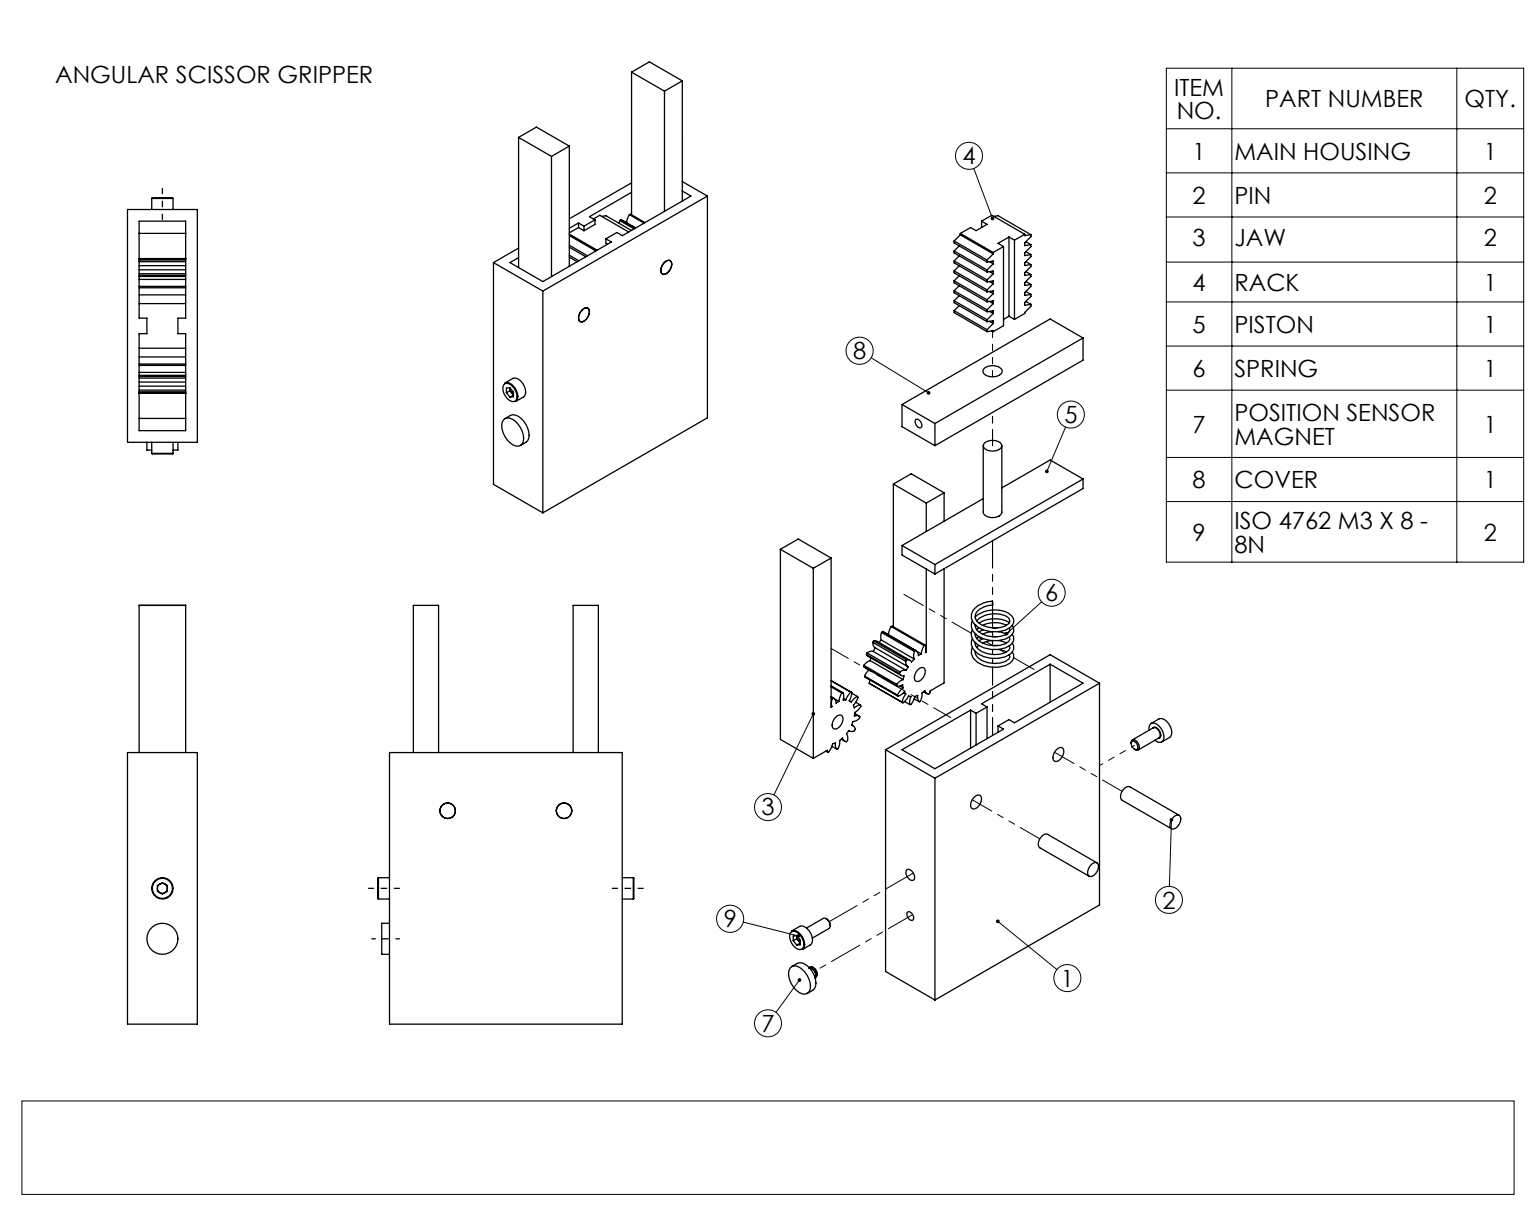
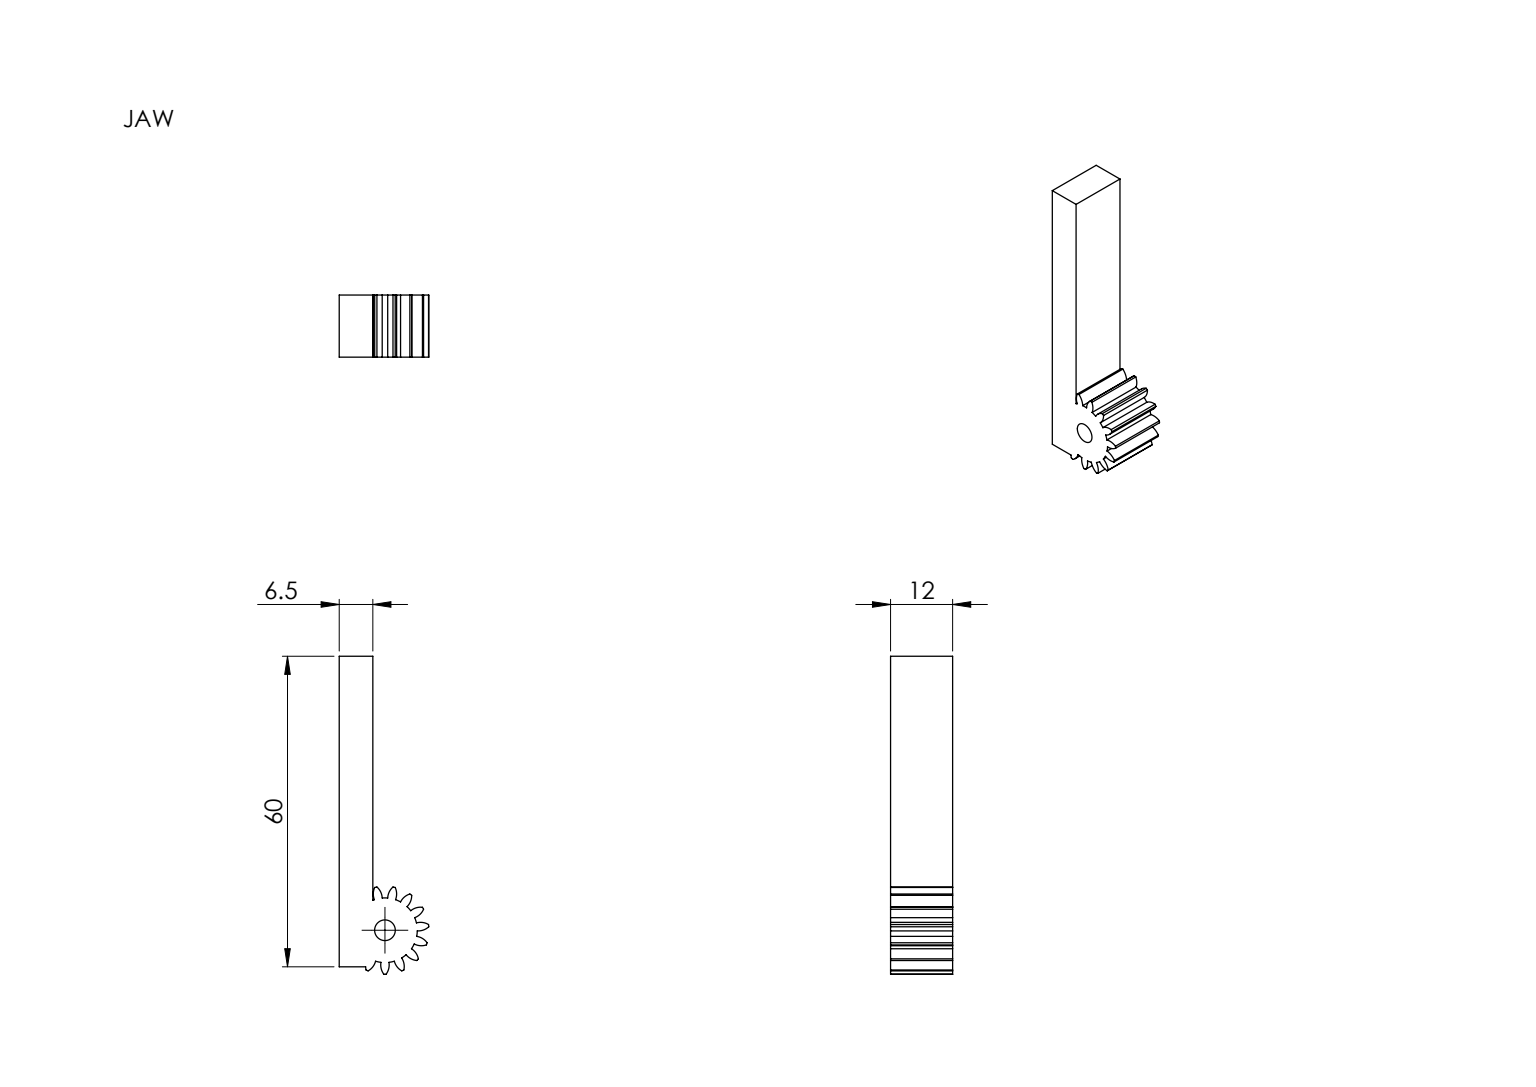
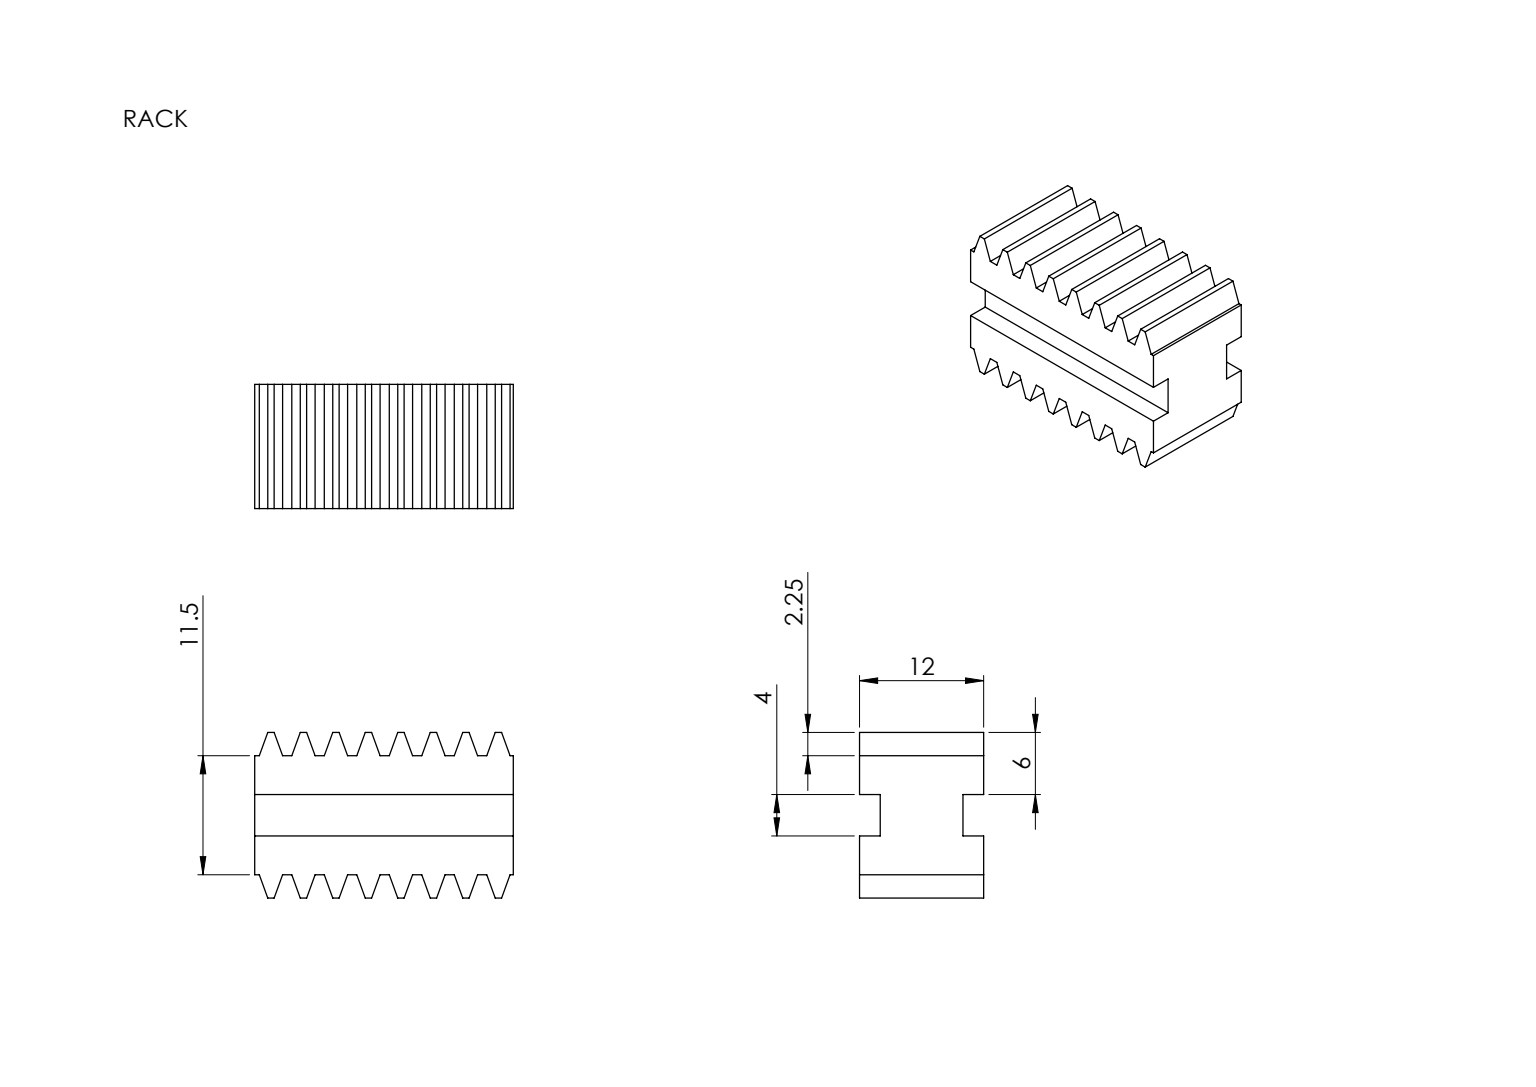
ISO-10303-21;
HEADER;
FILE_DESCRIPTION (('STEP AP214'),
    '1' );
FILE_NAME ('BR-002',
    '2026-10-03T18:28:46',
    ( '' ),
    ( '' ),
    'SwSTEP 2.0',
    'SolidWorks 2026',
    '' );
FILE_SCHEMA (( 'AUTOMOTIVE_DESIGN' ));
ENDSEC;

DATA;
#1 =( LENGTH_UNIT ( ) NAMED_UNIT ( * ) SI_UNIT ( .MILLI., .METRE. ) );
#2 = ORIENTED_EDGE ( 'NONE', *, *, #1158, .F. ) ;
#3 = DIRECTION ( 'NONE',  ( -1.000000000000000000, 0.000000000000000000, 0.000000000000000000 ) ) ;
#4 = DIRECTION ( 'NONE',  ( 0.000000000000000000, 0.000000000000000000, 1.000000000000000000 ) ) ;
#5 = DIRECTION ( 'NONE',  ( 0.3420201433256627732, 0.9396926207859105373, 0.000000000000000000 ) ) ;
#6 = CARTESIAN_POINT ( 'NONE',  ( 10.71950000000001424, 0.000000000000000000, 1.500000000000000222 ) ) ;
#7 = EDGE_CURVE ( 'NONE', #9588, #252, #7094, .T. ) ;
#8 = DIRECTION ( 'NONE',  ( 1.000000000000000000, -0.000000000000000000, -0.000000000000000000 ) ) ;
#9 = CARTESIAN_POINT ( 'NONE',  ( -2.231261971483764484, -4.173491630687871101, 3.063948283277976081 ) ) ;
#10 = ORIENTED_EDGE ( 'NONE', *, *, #5513, .T. ) ;
#11 = AXIS2_PLACEMENT_3D ( 'NONE', #9784, #8139, #4791 ) ;
#12 = PLANE ( 'NONE',  #9677 ) ;
#13 = SHAPE_REPRESENTATION ( 'piston', ( #2101 ), #6502 ) ;
#14 = CARTESIAN_POINT ( 'NONE',  ( 4.089228379062037178, -4.089228379062022967, 0.6999999999999997335 ) ) ;
#15 = DIRECTION ( 'NONE',  ( 0.000000000000000000, 1.000000000000000000, -1.320393690296331133E-15 ) ) ;
#16 = PRODUCT_CONTEXT ( 'NONE', #527, 'mechanical' ) ;
#17 = CIRCLE ( 'NONE', #8645, 6.248999999999999666 ) ;
#18 = CARTESIAN_POINT ( 'NONE',  ( 0.9046671180729953798, -5.711843387010016926, 0.9799999999999997602 ) ) ;
#19 = ADVANCED_FACE ( 'NONE', ( #1564 ), #26, .F. ) ;
#20 = CARTESIAN_POINT ( 'NONE',  ( -1.500000000000000222, -13.00000000000000533, -1.812500001365593416 ) ) ;
#21 = EDGE_CURVE ( 'NONE', #307, #4726, #872, .T. ) ;
#22 = DIRECTION ( 'NONE',  ( 0.000000000000000000, 0.000000000000000000, 1.000000000000000000 ) ) ;
#23 = EDGE_CURVE ( 'NONE', #8074, #935, #6750, .T. ) ;
#24 = LINE ( 'NONE', #5186, #1032 ) ;
#25 = VECTOR ( 'NONE', #10165, 1000.000000000000000 ) ;
#26 = PLANE ( 'NONE',  #10330 ) ;
#27 = AXIS2_PLACEMENT_3D ( 'NONE', #3264, #1729, #5737 ) ;
#28 = CARTESIAN_POINT ( 'NONE',  ( 8.000000000000001776, 7.008469740302810891, -0.7425307242147085596 ) ) ;
#29 = DIRECTION ( 'NONE',  ( -1.000000000000000000, -0.000000000000000000, -0.000000000000000000 ) ) ;
#30 = CARTESIAN_POINT ( 'NONE',  ( 1.963858260114715870, -4.049832306626327316, 5.443948283277975975 ) ) ;
#31 = VECTOR ( 'NONE', #1258, 1000.000000000000000 ) ;
#32 = CARTESIAN_POINT ( 'NONE',  ( -3.181725716174720498E-16, -14.73205080756888385, -1.125000000000000000 ) ) ;
#33 = EDGE_LOOP ( 'NONE', ( #1862, #211, #6876, #1898 ) ) ;
#34 = AXIS2_PLACEMENT_3D ( 'NONE', #10379, #6382, #8043 ) ;
#35 = ORIENTED_EDGE ( 'NONE', *, *, #573, .T. ) ;
#36 = EDGE_CURVE ( 'NONE', #3582, #9702, #3146, .T. ) ;
#37 = DIRECTION ( 'NONE',  ( 0.000000000000000000, 0.000000000000000000, 1.000000000000000000 ) ) ;
#38 = CARTESIAN_POINT ( 'NONE',  ( 7.054542135639013677E-15, -28.99999999999999289, 0.000000000000000000 ) ) ;
#39 = ORIENTED_EDGE ( 'NONE', *, *, #10148, .F. ) ;
#40 = CARTESIAN_POINT ( 'NONE',  ( 0.7401821875142697849, -4.673326407553650697, 3.779999999999998916 ) ) ;
#41 = FACE_OUTER_BOUND ( 'NONE', #7858, .T. ) ;
#42 = ORIENTED_EDGE ( 'NONE', *, *, #3976, .T. ) ;
#43 = CARTESIAN_POINT ( 'NONE',  ( -0.9968613283357868893, 5.697241258616382531, 14.57605171672202538 ) ) ;
#44 = ORIENTED_EDGE ( 'NONE', *, *, #5320, .F. ) ;
#45 = ORIENTED_EDGE ( 'NONE', *, *, #5401, .F. ) ;
#46 = FACE_OUTER_BOUND ( 'NONE', #10061, .T. ) ;
#47 = CARTESIAN_POINT ( 'NONE',  ( 1.229367062500000163, -13.00000000000000533, 0.2187499993172034862 ) ) ;
#48 = VERTEX_POINT ( 'NONE', #8977 ) ;
#49 = CARTESIAN_POINT ( 'NONE',  ( 5.432285873273257515, 0.8603895577212793411, 8.679999999999997939 ) ) ;
#50 = CARTESIAN_POINT ( 'NONE',  ( -2.000000000000000000, 4.137773741518453008, -5.705158055754754542 ) ) ;
#51 = CARTESIAN_POINT ( 'NONE',  ( -3.889087296526005044, -3.889087296526019255, 1.399999999999999689 ) ) ;
#52 = ORIENTED_EDGE ( 'NONE', *, *, #338, .F. ) ;
#53 = CARTESIAN_POINT ( 'NONE',  ( 1.060575238724907038E-16, -11.26794919243112680, 0.06249999863440621611 ) ) ;
#54 = APPLICATION_CONTEXT ( 'automotive_design' ) ;
#55 = ORIENTED_EDGE ( 'NONE', *, *, #4599, .F. ) ;
#56 = PRODUCT ( 'socket head cap screw_iso_ISO 4762 M3 x 8 - 8N', 'socket head cap screw_iso_ISO 4762 M3 x 8 - 8N', '', ( #8757 ) ) ;
#57 = FACE_OUTER_BOUND ( 'NONE', #643, .T. ) ;
#58 = CARTESIAN_POINT ( 'NONE',  ( 10.00000000000000000, 5.904264776415100613, 2.046865518294722630 ) ) ;
#59 = DIRECTION ( 'NONE',  ( 0.9396926207859105373, -0.3420201433256627732, 0.000000000000000000 ) ) ;
#60 = DIRECTION ( 'NONE',  ( 0.000000000000000000, 1.000000000000000000, -7.228014483236699822E-18 ) ) ;
#61 = CIRCLE ( 'NONE', #8365, 3.000000000000000000 ) ;
#62 = CARTESIAN_POINT ( 'NONE',  ( 15.26352788033274699, -7.750000000000000000, -12.00000000000000000 ) ) ;
#63 = EDGE_CURVE ( 'NONE', #2398, #931, #4099, .T. ) ;
#64 = CARTESIAN_POINT ( 'NONE',  ( 3.244753828200538148, 3.119207202478391672, -0.9960517167220231949 ) ) ;
#65 = VERTEX_POINT ( 'NONE', #8189 ) ;
#66 = CARTESIAN_POINT ( 'NONE',  ( 1.229367062500000385, -12.29022459553277002, -0.8020833340161301894 ) ) ;
#67 = CARTESIAN_POINT ( 'NONE',  ( -0.8603895577212598011, -5.432285873273260179, 6.719999999999999751 ) ) ;
#68 = DIRECTION ( 'NONE',  ( 0.000000000000000000, -0.000000000000000000, 1.000000000000000000 ) ) ;
#69 = ADVANCED_FACE ( 'NONE', ( #9627 ), #4044, .F. ) ;
#70 = CIRCLE ( 'NONE', #566, 8.500000000000000000 ) ;
#71 = CARTESIAN_POINT ( 'NONE',  ( 8.000000000000001776, -5.349675154362301122, -3.229702268444983648 ) ) ;
#72 = CARTESIAN_POINT ( 'NONE',  ( 8.161409553233806236, 6.000000000000000000, 0.000000000000000000 ) ) ;
#73 = CARTESIAN_POINT ( 'NONE',  ( 8.000000000000001776, -2.861184399890952079, -6.440778198864142823 ) ) ;
#74 = CARTESIAN_POINT ( 'NONE',  ( 4.414205890716556446, -10.02539999999999942, 0.000000000000000000 ) ) ;
#75 = DIRECTION ( 'NONE',  ( 1.000000000000000000, 0.000000000000000000, 0.000000000000000000 ) ) ;
#76 = CARTESIAN_POINT ( 'NONE',  ( 4.430710083317573655, 0.7916369971161595354, 1.276051716722023333 ) ) ;
#77 = SURFACE_STYLE_FILL_AREA ( #6636 ) ;
#78 = CARTESIAN_POINT ( 'NONE',  ( 11.30300220323380600, -10.00000000000000000, -12.00000000000000000 ) ) ;
#79 = CARTESIAN_POINT ( 'NONE',  ( 4.458484982038663169, 0.6162731882459350219, 2.083948283277976543 ) ) ;
#80 = PRODUCT_DEFINITION_CONTEXT ( 'detailed design', #6135, 'design' ) ;
#81 = EDGE_CURVE ( 'NONE', #3937, #2835, #7332, .T. ) ;
#82 = PLANE ( 'NONE',  #8867 ) ;
#83 = EDGE_CURVE ( 'NONE', #8159, #4280, #2511, .T. ) ;
#84 = ORIENTED_EDGE ( 'NONE', *, *, #6223, .T. ) ;
#85 = MECHANICAL_DESIGN_GEOMETRIC_PRESENTATION_REPRESENTATION (  '', ( #9215 ), #5323 ) ;
#86 = ORIENTED_EDGE ( 'NONE', *, *, #8247, .T. ) ;
#87 = CARTESIAN_POINT ( 'NONE',  ( 16.97133164676619899, -10.00000000000000000, -12.00000000000000000 ) ) ;
#88 = CARTESIAN_POINT ( 'NONE',  ( 0.000000000000000000, 52.93638525830372998, 8.843061888689529582 ) ) ;
#89 = ORIENTED_EDGE ( 'NONE', *, *, #4537, .T. ) ;
#90 = AXIS2_PLACEMENT_3D ( 'NONE', #8331, #4928, #5764 ) ;
#91 = CARTESIAN_POINT ( 'NONE',  ( 4.009529358847659708, -2.042957248827953709, 0.5599999999999999423 ) ) ;
#92 = ORIENTED_EDGE ( 'NONE', *, *, #6887, .T. ) ;
#93 = CARTESIAN_POINT ( 'NONE',  ( 4.430710083317573655, 0.7916369971161595354, 6.876051716722023421 ) ) ;
#94 = ADVANCED_FACE ( 'NONE', ( #8824 ), #10482, .F. ) ;
#95 = ORIENTED_EDGE ( 'NONE', *, *, #4515, .F. ) ;
#96 =( NAMED_UNIT ( * ) PLANE_ANGLE_UNIT ( ) SI_UNIT ( $, .RADIAN. ) );
#97 = VECTOR ( 'NONE', #1529, 1000.000000000000000 ) ;
#98 = ORIENTED_EDGE ( 'NONE', *, *, #3375, .T. ) ;
#99 = DIRECTION ( 'NONE',  ( -0.000000000000000000, -1.000000000000000000, -0.000000000000000000 ) ) ;
#100 = FILL_AREA_STYLE_COLOUR ( '', #7967 ) ;
#101 = ORIENTED_EDGE ( 'NONE', *, *, #1637, .T. ) ;
#102 = CARTESIAN_POINT ( 'NONE',  ( -3.889087296526005044, -3.889087296526019255, 4.200000000000000178 ) ) ;
#103 = CARTESIAN_POINT ( 'NONE',  ( 2.625446233515515537, 5.152728359536502545, 5.459999999999997300 ) ) ;
#104 = CARTESIAN_POINT ( 'NONE',  ( -5.697241258616385196, 0.9968613283357647958, 12.02394828327797427 ) ) ;
#105 = ORIENTED_EDGE ( 'NONE', *, *, #5645, .T. ) ;
#106 = CARTESIAN_POINT ( 'NONE',  ( 1.500000000000000222, -13.00000000000000533, -0.5625000013655934161 ) ) ;
#107 = ADVANCED_FACE ( 'NONE', ( #5725 ), #127, .T. ) ;
#108 = AXIS2_PLACEMENT_3D ( 'NONE', #9729, #5879, #8289 ) ;
#109 = ORIENTED_EDGE ( 'NONE', *, *, #1183, .T. ) ;
#110 = CARTESIAN_POINT ( 'NONE',  ( 5.999999999999999112, -27.00000000000000711, -14.00000000000000178 ) ) ;
#111 = CIRCLE ( 'NONE', #4663, 3.000000000000000000 ) ;
#112 = LINE ( 'NONE', #6402, #5089 ) ;
#113 = CARTESIAN_POINT ( 'NONE',  ( 1.060575238724907038E-16, -11.26794919243112680, -0.9375000013655935271 ) ) ;
#114 = CARTESIAN_POINT ( 'NONE',  ( 25.57717656966725883, -7.750000000000000000, -12.00000000000000000 ) ) ;
#115 = VECTOR ( 'NONE', #2977, 1000.000000000000000 ) ;
#116 = CARTESIAN_POINT ( 'NONE',  ( 0.6146835312500001924, -11.93533689329915326, -2.760416667349463449 ) ) ;
#117 = CARTESIAN_POINT ( 'NONE',  ( 0.7916369971161419938, 4.430710083317576320, 4.323948283277975868 ) ) ;
#118 = VERTEX_POINT ( 'NONE', #6579 ) ;
#119 = DIRECTION ( 'NONE',  ( 0.000000000000000000, 0.000000000000000000, 1.000000000000000000 ) ) ;
#120 = CARTESIAN_POINT ( 'NONE',  ( 4.089228379062037178, -4.089228379062022967, 9.099999999999999645 ) ) ;
#121 = CARTESIAN_POINT ( 'NONE',  ( 1.300000000000000044, -0.7390083445627200209, 1.280000000000001137 ) ) ;
#122 = CONTEXT_DEPENDENT_SHAPE_REPRESENTATION ( #7983, #5707 ) ;
#123 = CARTESIAN_POINT ( 'NONE',  ( 0.9046671180729953798, -5.711843387010016926, 9.379999999999997229 ) ) ;
#124 = CARTESIAN_POINT ( 'NONE',  ( 0.000000000000000000, 0.000000000000000000, -12.00000000000000000 ) ) ;
#125 = CARTESIAN_POINT ( 'NONE',  ( 30.00000000000001066, -34.99999999999999289, -9.000000000000000000 ) ) ;
#126 = PLANE ( 'NONE',  #1722 ) ;
#127 = CYLINDRICAL_SURFACE ( 'NONE', #2700, 1.500000000000000222 ) ;
#128 = CARTESIAN_POINT ( 'NONE',  ( 3.826313983664925811, 3.951860609387098044, 14.99605171672202175 ) ) ;
#129 = ADVANCED_FACE ( 'NONE', ( #8084 ), #5628, .T. ) ;
#130 = DIRECTION ( 'NONE',  ( 0.000000000000000000, 0.000000000000000000, -1.000000000000000000 ) ) ;
#131 = CARTESIAN_POINT ( 'NONE',  ( -4.258245684917310925, -2.064922774268914019, 6.143948283277977040 ) ) ;
#132 = LINE ( 'NONE', #5884, #6142 ) ;
#133 = ORIENTED_EDGE ( 'NONE', *, *, #9091, .T. ) ;
#134 = CARTESIAN_POINT ( 'NONE',  ( -0.9968613283357868893, 5.697241258616382531, 6.176051716722023244 ) ) ;
#135 = ORIENTED_EDGE ( 'NONE', *, *, #264, .F. ) ;
#136 = FACE_OUTER_BOUND ( 'NONE', #5788, .T. ) ;
#137 = DIRECTION ( 'NONE',  ( 5.204170427930421283E-15, 6.018531076210112041E-31, 1.000000000000000000 ) ) ;
#138 = VERTEX_POINT ( 'NONE', #1768 ) ;
#139 = CARTESIAN_POINT ( 'NONE',  ( 4.215868657802586128, 2.148092372876346801, 5.739999999999998437 ) ) ;
#140 = LINE ( 'NONE', #6544, #6932 ) ;
#141 = EDGE_LOOP ( 'NONE', ( #4012, #8680, #9261, #9381 ) ) ;
#142 = CARTESIAN_POINT ( 'NONE',  ( 3.411736077305382420, -3.279728542977940364, 7.296051716722023350 ) ) ;
#143 = CARTESIAN_POINT ( 'NONE',  ( 1.500000000000000222, -13.00000000000000533, 0.000000000000000000 ) ) ;
#144 = VERTEX_POINT ( 'NONE', #4838 ) ;
#145 = VERTEX_POINT ( 'NONE', #7277 ) ;
#146 = CARTESIAN_POINT ( 'NONE',  ( 12.12193523033274545, 3.750000000000000000, 0.000000000000000000 ) ) ;
#147 = ORIENTED_EDGE ( 'NONE', *, *, #2859, .T. ) ;
#148 = ADVANCED_FACE ( 'NONE', ( #6475 ), #9031, .T. ) ;
#149 = CARTESIAN_POINT ( 'NONE',  ( 3.889087296526005488, 3.889087296526018811, 5.599999999999998757 ) ) ;
#150 = EDGE_CURVE ( 'NONE', #6457, #8930, #2463, .T. ) ;
#151 = CARTESIAN_POINT ( 'NONE',  ( 5.432285873273257515, 0.8603895577212793411, 3.079999999999999627 ) ) ;
#152 = CARTESIAN_POINT ( 'NONE',  ( -5.152728359536494551, -2.625446233515535077, 1.540000000000000036 ) ) ;
#153 = EDGE_LOOP ( 'NONE', ( #2602, #8122, #9695, #3573 ) ) ;
#154 = DIRECTION ( 'NONE',  ( 1.000000000000000000, 0.000000000000000000, 0.000000000000000000 ) ) ;
#155 = AXIS2_PLACEMENT_3D ( 'NONE', #4132, #7961, #9612 ) ;
#156 = ORIENTED_EDGE ( 'NONE', *, *, #9552, .F. ) ;
#157 = CARTESIAN_POINT ( 'NONE',  ( 0.000000000000000000, 0.000000000000000000, 6.999999999999999112 ) ) ;
#158 = DIRECTION ( 'NONE',  ( -1.000000000000000000, -0.000000000000000000, -0.000000000000000000 ) ) ;
#159 = CARTESIAN_POINT ( 'NONE',  ( 1.999999999999987121, 15.00000000000000355, 4.000000000000008882 ) ) ;
#160 = ORIENTED_EDGE ( 'NONE', *, *, #6778, .T. ) ;
#161 = ADVANCED_FACE ( 'NONE', ( #10045 ), #7492, .F. ) ;
#162 = LINE ( 'NONE', #5033, #9824 ) ;
#163 = CARTESIAN_POINT ( 'NONE',  ( 1.229367062500000163, -13.00000000000000533, -0.3437500006827965970 ) ) ;
#164 = CARTESIAN_POINT ( 'NONE',  ( -4.215868657802586128, -2.148092372876348133, 12.73999999999999488 ) ) ;
#165 = VERTEX_POINT ( 'NONE', #5934 ) ;
#166 = MECHANICAL_DESIGN_GEOMETRIC_PRESENTATION_REPRESENTATION (  '', ( #664 ), #9477 ) ;
#167 = LINE ( 'NONE', #2277, #6439 ) ;
#168 = CIRCLE ( 'NONE', #6585, 2.999999999999999112 ) ;
#169 = CARTESIAN_POINT ( 'NONE',  ( -0.8603895577212598011, -5.432285873273260179, 1.119999999999999885 ) ) ;
#170 = CARTESIAN_POINT ( 'NONE',  ( 5.019816903233806471, 6.000000000000000000, -12.00000000000000000 ) ) ;
#171 = VECTOR ( 'NONE', #6634, 1000.000000000000000 ) ;
#172 = CARTESIAN_POINT ( 'NONE',  ( 0.9046671180729953798, -5.711843387010016926, 3.779999999999998916 ) ) ;
#173 = VECTOR ( 'NONE', #7941, 1000.000000000000000 ) ;
#174 = CARTESIAN_POINT ( 'NONE',  ( 8.000000000000001776, 5.241389472434725860, -4.711457988287000909 ) ) ;
#175 = PRESENTATION_LAYER_ASSIGNMENT (  '', '', ( #3720 ) ) ;
#176 = LINE ( 'NONE', #3458, #275 ) ;
#177 = CARTESIAN_POINT ( 'NONE',  ( 10.00000000000000000, -5.233522515400119701, 4.720195129223260899 ) ) ;
#178 = CARTESIAN_POINT ( 'NONE',  ( -5.418398423912711870, -0.9480714621563917088, 13.87605171672202253 ) ) ;
#179 = CARTESIAN_POINT ( 'NONE',  ( 1.300000000000000044, 0.000000000000000000, 0.000000000000000000 ) ) ;
#180 = PRODUCT_RELATED_PRODUCT_CATEGORY ( 'part', '', ( #8938 ) ) ;
#181 = VECTOR ( 'NONE', #6809, 1000.000000000000000 ) ;
#182 = CARTESIAN_POINT ( 'NONE',  ( -4.458484982038663169, -0.6162731882459353550, 9.083948283277974767 ) ) ;
#183 = AXIS2_PLACEMENT_3D ( 'NONE', #2466, #1616, #8926 ) ;
#184 = DIRECTION ( 'NONE',  ( -0.000000000000000000, -0.000000000000000000, -1.000000000000000000 ) ) ;
#186 = ORIENTED_EDGE ( 'NONE', *, *, #3227, .F. ) ;
#185 = AXIS2_PLACEMENT_3D ( 'NONE', #7791, #8589, #2122 ) ;
#187 = CARTESIAN_POINT ( 'NONE',  ( 3.826313983664925811, 3.951860609387098044, 0.9960517167220231949 ) ) ;
#188 = AXIS2_PLACEMENT_3D ( 'NONE', #2496, #158, #4930 ) ;
#189 = DIRECTION ( 'NONE',  ( 1.000000000000000000, 1.156482317317871478E-16, 5.637851296924623057E-15 ) ) ;
#190 = CIRCLE ( 'NONE', #4074, 3.000000000000000000 ) ;
#191 = CARTESIAN_POINT ( 'NONE',  ( 1.300000000000000044, -1.108512516844081475, 0.6400000000000016787 ) ) ;
#192 = ORIENTED_EDGE ( 'NONE', *, *, #4599, .T. ) ;
#193 = CARTESIAN_POINT ( 'NONE',  ( 4.673326407553653361, -0.7401821875142525764, 0.4199999999999999845 ) ) ;
#194 =( REPRESENTATION_RELATIONSHIP ('NONE','NONE', #5100, #7954 ) REPRESENTATION_RELATIONSHIP_WITH_TRANSFORMATION ( #1761 )SHAPE_REPRESENTATION_RELATIONSHIP( ) );
#195 = CIRCLE ( 'NONE', #5093, 3.000000000000000000 ) ;
#196 = CARTESIAN_POINT ( 'NONE',  ( 8.000000000000001776, -4.724769925181144359, -4.089810527897808079 ) ) ;
#197 = ORIENTED_EDGE ( 'NONE', *, *, #1437, .F. ) ;
#198 = CARTESIAN_POINT ( 'NONE',  ( 4.687928535947288644, -0.6479879772514620662, 4.216051716722023279 ) ) ;
#199 = VECTOR ( 'NONE', #189, 1000.000000000000000 ) ;
#200 = CARTESIAN_POINT ( 'NONE',  ( 1.530808498934188612E-16, 18.99999999999999289, -1.249999999999997558 ) ) ;
#201 = VERTEX_POINT ( 'NONE', #9239 ) ;
#202 = CARTESIAN_POINT ( 'NONE',  ( 0.000000000000000000, 0.000000000000000000, 0.000000000000000000 ) ) ;
#203 = EDGE_CURVE ( 'NONE', #3477, #3593, #1173, .T. ) ;
#204 = ORIENTED_EDGE ( 'NONE', *, *, #9490, .F. ) ;
#205 = DIRECTION ( 'NONE',  ( 0.000000000000000000, 0.000000000000000000, 1.000000000000000000 ) ) ;
#206 = CYLINDRICAL_SURFACE ( 'NONE', #9839, 1.500000000000000222 ) ;
#207 = ORIENTED_EDGE ( 'NONE', *, *, #5389, .F. ) ;
#208 = CARTESIAN_POINT ( 'NONE',  ( -4.089228379062038066, 4.089228379062021190, 13.29999999999999538 ) ) ;
#209 = CARTESIAN_POINT ( 'NONE',  ( -4.900535883036028828, 2.496947748567499126, 4.759999999999999787 ) ) ;
#210 = CARTESIAN_POINT ( 'NONE',  ( -5.711843387010018702, 0.9046671180729746187, 1.819999999999999396 ) ) ;
#211 = ORIENTED_EDGE ( 'NONE', *, *, #1815, .F. ) ;
#212 = CARTESIAN_POINT ( 'NONE',  ( -2.607672531582950546E-16, -14.41955080893447416, -0.3437500006827965415 ) ) ;
#213 = EDGE_CURVE ( 'NONE', #3364, #1830, #6075, .T. ) ;
#214 = FILL_AREA_STYLE_COLOUR ( '', #3785 ) ;
#215 = EDGE_CURVE ( 'NONE', #8955, #6611, #5198, .T. ) ;
#216 = VERTEX_POINT ( 'NONE', #1872 ) ;
#217 = DIRECTION ( 'NONE',  ( 1.000000000000000000, 0.000000000000000000, 0.000000000000000000 ) ) ;
#218 = CARTESIAN_POINT ( 'NONE',  ( 4.000000000000000888, 8.357095590591340439, -1.552080310331536372 ) ) ;
#219 = DIRECTION ( 'NONE',  ( -1.000000000000000000, -0.000000000000000000, -0.000000000000000000 ) ) ;
#220 = ORIENTED_EDGE ( 'NONE', *, *, #9750, .F. ) ;
#221 = DIRECTION ( 'NONE',  ( -0.000000000000000000, -0.000000000000000000, 1.000000000000000000 ) ) ;
#222 = CARTESIAN_POINT ( 'NONE',  ( -1.229367062500000163, -13.70977540446723708, -1.052083334016129967 ) ) ;
#223 = CARTESIAN_POINT ( 'NONE',  ( -1.963858260114716980, 4.049832306626327316, 1.243948283277976463 ) ) ;
#224 = ORIENTED_EDGE ( 'NONE', *, *, #10008, .F. ) ;
#225 = CYLINDRICAL_SURFACE ( 'NONE', #1715, 2.500000000000000000 ) ;
#226 = CARTESIAN_POINT ( 'NONE',  ( 2.496947748567516889, -4.900535883036019946, 6.439999999999999503 ) ) ;
#227 = EDGE_CURVE ( 'NONE', #7607, #7874, #10094, .T. ) ;
#228 = DIRECTION ( 'NONE',  ( 1.000000000000000000, 0.000000000000000000, -0.000000000000000000 ) ) ;
#229 = CARTESIAN_POINT ( 'NONE',  ( 0.8603895577212593571, 5.432285873273261068, 5.319999999999999396 ) ) ;
#230 = VECTOR ( 'NONE', #6076, 1000.000000000000000 ) ;
#231 = PLANE ( 'NONE',  #1121 ) ;
#232 = LINE ( 'NONE', #7430, #6006 ) ;
#233 = EDGE_CURVE ( 'NONE', #10188, #6283, #1978, .T. ) ;
#234 = DIRECTION ( 'NONE',  ( -1.000000000000000000, -0.000000000000000000, -0.000000000000000000 ) ) ;
#235 = CARTESIAN_POINT ( 'NONE',  ( 4.173491630687861331, 2.231261971483781359, 1.136051716722023208 ) ) ;
#236 = DIRECTION ( 'NONE',  ( -0.000000000000000000, -0.000000000000000000, 1.000000000000000000 ) ) ;
#237 = CARTESIAN_POINT ( 'NONE',  ( -1.963858260114716980, 4.049832306626327316, 4.043948283277976508 ) ) ;
#238 = AXIS2_PLACEMENT_3D ( 'NONE', #8296, #9037, #6583 ) ;
#239 = CARTESIAN_POINT ( 'NONE',  ( 9.000000000000000000, 19.99999999999999645, 13.00000000000000000 ) ) ;
#240 = ORIENTED_EDGE ( 'NONE', *, *, #4869, .F. ) ;
#241 = CARTESIAN_POINT ( 'NONE',  ( 4.155232146225751322, -4.023224611898307934, 7.296051716722023350 ) ) ;
#242 = DIRECTION ( 'NONE',  ( 0.9396926207859105373, 0.3420201433256627732, 0.000000000000000000 ) ) ;
#243 = CARTESIAN_POINT ( 'NONE',  ( 5.010572059283444624, 6.025400000000000311, -12.00000000000000000 ) ) ;
#244 = VERTEX_POINT ( 'NONE', #6788 ) ;
#245 = CARTESIAN_POINT ( 'NONE',  ( 4.673326407553653361, -0.7401821875142525764, 11.61999999999999922 ) ) ;
#246 = LINE ( 'NONE', #6800, #847 ) ;
#247 = VERTEX_POINT ( 'NONE', #6726 ) ;
#248 = CARTESIAN_POINT ( 'NONE',  ( -4.173491630687863108, -2.231261971483782691, 10.93605171672202125 ) ) ;
#249 = DIRECTION ( 'NONE',  ( -1.000000000000000000, 0.000000000000000000, 0.000000000000000000 ) ) ;
#250 = ORIENTED_EDGE ( 'NONE', *, *, #7768, .T. ) ;
#251 =( LENGTH_UNIT ( ) NAMED_UNIT ( * ) SI_UNIT ( .MILLI., .METRE. ) );
#252 = VERTEX_POINT ( 'NONE', #2821 ) ;
#253 = EDGE_CURVE ( 'NONE', #3846, #7785, #9133, .T. ) ;
#254 = CARTESIAN_POINT ( 'NONE',  ( 8.000000000000001776, 0.000000000000000000, 0.000000000000000000 ) ) ;
#255 =( NAMED_UNIT ( * ) SI_UNIT ( $, .STERADIAN. ) SOLID_ANGLE_UNIT ( ) );
#256 = ORIENTED_EDGE ( 'NONE', *, *, #1778, .T. ) ;
#257 = CARTESIAN_POINT ( 'NONE',  ( 0.7727076532861471003, 5.446173322633805824, 3.516051716722023102 ) ) ;
#258 = FACE_OUTER_BOUND ( 'NONE', #8568, .T. ) ;
#259 = STYLED_ITEM ( 'NONE', ( #1415 ), #6736 ) ;
#260 = VECTOR ( 'NONE', #2715, 1000.000000000000000 ) ;
#261 = CARTESIAN_POINT ( 'NONE',  ( 3.889087296526005488, 3.889087296526018811, 11.19999999999999751 ) ) ;
#262 = EDGE_LOOP ( 'NONE', ( #2145, #5885, #3192, #5080 ) ) ;
#263 = CARTESIAN_POINT ( 'NONE',  ( -2.607672531582950546E-16, -14.41955080893447416, -1.343750000682796708 ) ) ;
#264 = EDGE_CURVE ( 'NONE', #5062, #6335, #3411, .T. ) ;
#265 = VECTOR ( 'NONE', #8626, 1000.000000000000000 ) ;
#266 = ORIENTED_EDGE ( 'NONE', *, *, #5238, .F. ) ;
#267 = CARTESIAN_POINT ( 'NONE',  ( 25.00000000000000000, -4.000000000000000000, -12.00000000000000000 ) ) ;
#268 = LINE ( 'NONE', #4231, #6080 ) ;
#269 = ORIENTED_EDGE ( 'NONE', *, *, #2906, .F. ) ;
#270 = CARTESIAN_POINT ( 'NONE',  ( 0.000000000000000000, 6.000000000000000000, 0.000000000000000000 ) ) ;
#271 = VECTOR ( 'NONE', #4642, 1000.000000000000000 ) ;
#272 = CARTESIAN_POINT ( 'NONE',  ( -1.229367062500000163, -13.00000000000000533, -0.5937500006827968191 ) ) ;
#273 = CARTESIAN_POINT ( 'NONE',  ( -2.231261971483764484, -4.173491630687871101, 5.863948283277976792 ) ) ;
#274 = VERTEX_POINT ( 'NONE', #5981 ) ;
#275 = VECTOR ( 'NONE', #4885, 1000.000000000000000 ) ;
#276 = DIRECTION ( 'NONE',  ( 1.000000000000000000, 0.000000000000000000, 0.000000000000000000 ) ) ;
#277 = ADVANCED_FACE ( 'NONE', ( #8443 ), #9887, .T. ) ;
#278 = PLANE ( 'NONE',  #8859 ) ;
#279 = CARTESIAN_POINT ( 'NONE',  ( 0.9270509719278221539, -11.80318232062615991, 0.01099716686063855267 ) ) ;
#280 = AXIS2_PLACEMENT_3D ( 'NONE', #7224, #4941, #9679 ) ;
#281 = CARTESIAN_POINT ( 'NONE',  ( -2.625446233515515537, -5.152728359536502545, 9.659999999999996589 ) ) ;
#282 = VECTOR ( 'NONE', #6359, 1000.000000000000000 ) ;
#283 = FACE_OUTER_BOUND ( 'NONE', #3268, .T. ) ;
#284 = DIRECTION ( 'NONE',  ( -1.000000000000000000, -0.000000000000000000, -0.000000000000000000 ) ) ;
#285 = DIRECTION ( 'NONE',  ( 0.000000000000000000, 0.000000000000000000, 1.000000000000000000 ) ) ;
#286 = CARTESIAN_POINT ( 'NONE',  ( -4.687928535947287756, 0.6479879772514611780, 8.416051716722021681 ) ) ;
#287 = EDGE_CURVE ( 'NONE', #717, #2796, #5043, .T. ) ;
#288 = ADVANCED_FACE ( 'NONE', ( #384 ), #8291, .T. ) ;
#289 = CARTESIAN_POINT ( 'NONE',  ( -1.229367062500000163, -13.00000000000000533, -1.468750000682796486 ) ) ;
#290 = CARTESIAN_POINT ( 'NONE',  ( -4.860232935257354114, 2.576046737280751842, 0.9639482832779766586 ) ) ;
#291 = DIRECTION ( 'NONE',  ( -1.000000000000000000, -0.000000000000000000, -0.000000000000000000 ) ) ;
#292 = VERTEX_POINT ( 'NONE', #4247 ) ;
#293 = CARTESIAN_POINT ( 'NONE',  ( -0.7727076532861475444, -5.446173322633804048, 7.716051716722023279 ) ) ;
#294 = DIRECTION ( 'NONE',  ( 0.000000000000000000, 0.000000000000000000, -1.000000000000000000 ) ) ;
#295 = PLANE ( 'NONE',  #8652 ) ;
#296 = ORIENTED_EDGE ( 'NONE', *, *, #1709, .F. ) ;
#297 = EDGE_CURVE ( 'NONE', #931, #7411, #3459, .T. ) ;
#298 = CARTESIAN_POINT ( 'NONE',  ( -2.148092372876330813, -4.215868657802594122, 6.859999999999999432 ) ) ;
#299 =( NAMED_UNIT ( * ) SI_UNIT ( $, .STERADIAN. ) SOLID_ANGLE_UNIT ( ) );
#300 = CARTESIAN_POINT ( 'NONE',  ( -4.173491630687863108, -2.231261971483782691, 8.136051716722024096 ) ) ;
#301 = CARTESIAN_POINT ( 'NONE',  ( -1.229367062500000163, -13.00000000000000533, -2.593750000682796486 ) ) ;
#302 = ORIENTED_EDGE ( 'NONE', *, *, #6506, .F. ) ;
#303 = DIRECTION ( 'NONE',  ( -1.000000000000000000, -8.326672684688151433E-17, 3.399086336214591434E-19 ) ) ;
#304 = ORIENTED_EDGE ( 'NONE', *, *, #4469, .T. ) ;
#305 = CARTESIAN_POINT ( 'NONE',  ( -2.000000000000000000, -2.861184399890952079, -6.440778198864142823 ) ) ;
#306 = FACE_BOUND ( 'NONE', #5426, .T. ) ;
#307 = VERTEX_POINT ( 'NONE', #8395 ) ;
#308 = CARTESIAN_POINT ( 'NONE',  ( 5.432285873273257515, 0.8603895577212793411, 11.47999999999999865 ) ) ;
#309 = CARTESIAN_POINT ( 'NONE',  ( 3.889087296526005488, 3.889087296526018811, 2.799999999999999378 ) ) ;
#310 = CARTESIAN_POINT ( 'NONE',  ( 4.089228379062037178, -4.089228379062022967, 11.90000000000000036 ) ) ;
#311 = EDGE_LOOP ( 'NONE', ( #449, #2452, #4667, #4816 ) ) ;
#312 = CARTESIAN_POINT ( 'NONE',  ( 8.692241771943169307E-17, -11.58044919106553294, -0.09375000068279677745 ) ) ;
#313 = PRODUCT_DEFINITION_SHAPE ( 'NONE', 'NONE',  #10507 ) ;
#314 = ORIENTED_EDGE ( 'NONE', *, *, #8184, .T. ) ;
#315 = CARTESIAN_POINT ( 'NONE',  ( 19.29399126966725575, -7.750000000000000000, -12.00000000000000000 ) ) ;
#316 = PLANE ( 'NONE',  #9995 ) ;
#317 = VERTEX_POINT ( 'NONE', #6837 ) ;
#318 = DIRECTION ( 'NONE',  ( -0.000000000000000000, -1.000000000000000000, -0.000000000000000000 ) ) ;
#319 = FACE_OUTER_BOUND ( 'NONE', #4764, .T. ) ;
#320 = CARTESIAN_POINT ( 'NONE',  ( -2.607672531582950546E-16, -14.41955080893447416, -0.4687500006827967081 ) ) ;
#321 = CARTESIAN_POINT ( 'NONE',  ( 3.969226411068985882, -2.122056237541205981, 10.76394828327797626 ) ) ;
#322 = ORIENTED_EDGE ( 'NONE', *, *, #3486, .F. ) ;
#323 = PLANE ( 'NONE',  #6266 ) ;
#324 = CIRCLE ( 'NONE', #7596, 1.280000000000000027 ) ;
#325 = CARTESIAN_POINT ( 'NONE',  ( -2.625446233515515981, -5.152728359536500768, 12.45999999999999552 ) ) ;
#326 = DIRECTION ( 'NONE',  ( 0.000000000000000000, 0.000000000000000000, -1.000000000000000000 ) ) ;
#327 = CARTESIAN_POINT ( 'NONE',  ( -2.496947748567517333, 4.900535883036019058, 7.839999999999999858 ) ) ;
#328 = EDGE_CURVE ( 'NONE', #7607, #1777, #2963, .T. ) ;
#329 = FACE_OUTER_BOUND ( 'NONE', #5922, .T. ) ;
#330 = DIRECTION ( 'NONE',  ( -1.000000000000000000, -0.000000000000000000, -0.000000000000000000 ) ) ;
#331 = DIRECTION ( 'NONE',  ( -1.000000000000000000, -4.625929269271485914E-16, 0.000000000000000000 ) ) ;
#332 = CARTESIAN_POINT ( 'NONE',  ( 0.6162731882459174804, 4.458484982038668498, 11.91605171672202346 ) ) ;
#333 = AXIS2_PLACEMENT_3D ( 'NONE', #1807, #5615, #7419 ) ;
#334 = CARTESIAN_POINT ( 'NONE',  ( 1.229367062499999719, -13.70977540446724063, -2.260416667349463005 ) ) ;
#335 = CARTESIAN_POINT ( 'NONE',  ( 0.8124729078102063129, -5.726445515403652209, -0.01605171672202330979 ) ) ;
#336 = CARTESIAN_POINT ( 'NONE',  ( -2.607672531582950546E-16, -14.41955080893447416, -0.3437500006827965415 ) ) ;
#337 = AXIS2_PLACEMENT_3D ( 'NONE', #4333, #7524, #4129 ) ;
#338 = EDGE_CURVE ( 'NONE', #7188, #9680, #5880, .T. ) ;
#339 = ORIENTED_EDGE ( 'NONE', *, *, #9880, .F. ) ;
#340 = ADVANCED_FACE ( 'NONE', ( #9129 ), #3510, .F. ) ;
#341 = VECTOR ( 'NONE', #1990, 1000.000000000000000 ) ;
#342 = CARTESIAN_POINT ( 'NONE',  ( 3.889087296526005488, 3.889087296526018811, 13.99999999999999822 ) ) ;
#343 = EDGE_CURVE ( 'NONE', #9521, #8355, #5353, .T. ) ;
#344 = CYLINDRICAL_SURFACE ( 'NONE', #7027, 8.500000000000000000 ) ;
#345 = LINE ( 'NONE', #6849, #7114 ) ;
#346 = VERTEX_POINT ( 'NONE', #10198 ) ;
#347 = AXIS2_PLACEMENT_3D ( 'NONE', #3685, #9425, #2154 ) ;
#348 = CARTESIAN_POINT ( 'NONE',  ( 2.042957248827968808, -4.009529358847652603, 6.439999999999999503 ) ) ;
#349 = DIRECTION ( 'NONE',  ( -0.000000000000000000, -1.000000000000000000, -0.000000000000000000 ) ) ;
#350 = CARTESIAN_POINT ( 'NONE',  ( -4.009529358847660596, 2.042957248827953265, 1.959999999999999964 ) ) ;
#351 = CARTESIAN_POINT ( 'NONE',  ( -0.6146835312500006365, -14.06466310670085562, -0.01041666734946352160 ) ) ;
#352 = ORIENTED_EDGE ( 'NONE', *, *, #7205, .T. ) ;
#353 = EDGE_CURVE ( 'NONE', #8450, #9806, #2322, .T. ) ;
#354 = VECTOR ( 'NONE', #1516, 1000.000000000000000 ) ;
#355 = EDGE_LOOP ( 'NONE', ( #1789, #5959, #4901, #4754 ) ) ;
#356 = DIRECTION ( 'NONE',  ( 0.000000000000000000, 0.000000000000000000, 1.000000000000000000 ) ) ;
#357 = AXIS2_PLACEMENT_3D ( 'NONE', #179, #3413, #5576 ) ;
#358 = DIRECTION ( 'NONE',  ( 0.000000000000000000, 0.000000000000000000, 1.000000000000000000 ) ) ;
#359 = ORIENTED_EDGE ( 'NONE', *, *, #10190, .F. ) ;
#360 = CARTESIAN_POINT ( 'NONE',  ( -0.7727076532861475444, -5.446173322633804048, 2.116051716722023190 ) ) ;
#361 = CARTESIAN_POINT ( 'NONE',  ( -0.8603895577212598011, -5.432285873273260179, 12.31999999999999851 ) ) ;
#362 = CIRCLE ( 'NONE', #3066, 1.500000000000000222 ) ;
#363 = CARTESIAN_POINT ( 'NONE',  ( -5.152728359536494551, -2.625446233515535077, 7.139999999999997016 ) ) ;
#364 = ORIENTED_EDGE ( 'NONE', *, *, #1850, .F. ) ;
#365 = AXIS2_PLACEMENT_3D ( 'NONE', #4043, #10034, #4146 ) ;
#366 = CARTESIAN_POINT ( 'NONE',  ( 1.229367062500000163, -13.00000000000000533, -2.218750000682796486 ) ) ;
#367 = EDGE_LOOP ( 'NONE', ( #135, #7776, #8041, #9114 ) ) ;
#368 = CARTESIAN_POINT ( 'NONE',  ( 3.099999999999998757, 1.836970198721030181E-16, -1.500000000000000222 ) ) ;
#369 = CARTESIAN_POINT ( 'NONE',  ( 6.727620669667255804, -7.750000000000000000, 0.000000000000000000 ) ) ;
#370 = PRODUCT_RELATED_PRODUCT_CATEGORY ( 'part', '', ( #56 ) ) ;
#371 = VERTEX_POINT ( 'NONE', #1326 ) ;
#372 = CARTESIAN_POINT ( 'NONE',  ( 18.40512053033274853, 3.750000000000000000, -12.00000000000000000 ) ) ;
#373 = DIRECTION ( 'NONE',  ( 1.000000000000000000, -0.000000000000000000, -0.000000000000000000 ) ) ;
#374 = CARTESIAN_POINT ( 'NONE',  ( -1.229367062500000163, -12.29022459553277002, -2.635416667349463449 ) ) ;
#375 = CARTESIAN_POINT ( 'NONE',  ( 3.279728542977952799, -3.411736077305369541, 10.90394828327797327 ) ) ;
#376 = VERTEX_POINT ( 'NONE', #586 ) ;
#377 = DIRECTION ( 'NONE',  ( 0.9396926207859105373, -0.3420201433256627732, 0.000000000000000000 ) ) ;
#378 = CARTESIAN_POINT ( 'NONE',  ( 2.496947748567516889, -4.900535883036019946, 12.03999999999999915 ) ) ;
#379 = CARTESIAN_POINT ( 'NONE',  ( 9.869213319667256457, -7.750000000000000000, -12.00000000000000000 ) ) ;
#380 = DIRECTION ( 'NONE',  ( 0.000000000000000000, 0.000000000000000000, 1.000000000000000000 ) ) ;
#381 = DIRECTION ( 'NONE',  ( 1.000000000000000000, 0.000000000000000000, 0.000000000000000000 ) ) ;
#382 = EDGE_CURVE ( 'NONE', #3846, #7164, #6301, .T. ) ;
#383 = DIRECTION ( 'NONE',  ( 0.000000000000000000, 0.000000000000000000, 1.000000000000000000 ) ) ;
#384 = FACE_OUTER_BOUND ( 'NONE', #2361, .T. ) ;
#385 = CARTESIAN_POINT ( 'NONE',  ( -4.430710083317573655, -0.7916369971161599794, 11.07605171672202182 ) ) ;
#386 = CARTESIAN_POINT ( 'NONE',  ( 15.00000000000000000, 19.99999999999999645, -9.000000000000000000 ) ) ;
#387 = EDGE_CURVE ( 'NONE', #1597, #8333, #6145, .T. ) ;
#388 = CARTESIAN_POINT ( 'NONE',  ( -5.446173322633801384, -0.7727076532861678615, 0.6839482832779766319 ) ) ;
#389 = CARTESIAN_POINT ( 'NONE',  ( 1.229367062500000163, -13.00000000000000533, -1.718750000682796486 ) ) ;
#390 = ORIENTED_EDGE ( 'NONE', *, *, #4857, .T. ) ;
#391 = VECTOR ( 'NONE', #4021, 1000.000000000000000 ) ;
#392 = FACE_OUTER_BOUND ( 'NONE', #3063, .T. ) ;
#393 = CARTESIAN_POINT ( 'NONE',  ( 5.999999999999999112, -27.00000000000000711, -4.000000000000000000 ) ) ;
#394 = CARTESIAN_POINT ( 'NONE',  ( 25.00000000000000000, 0.000000000000000000, -12.00000000000000000 ) ) ;
#395 = ORIENTED_EDGE ( 'NONE', *, *, #7205, .F. ) ;
#396 = CARTESIAN_POINT ( 'NONE',  ( -0.7039550926810301812, -4.444597532678121965, 12.31999999999999851 ) ) ;
#397 = AXIS2_PLACEMENT_3D ( 'NONE', #6365, #7050, #5039 ) ;
#398 = EDGE_CURVE ( 'NONE', #7355, #525, #6229, .T. ) ;
#399 = ADVANCED_FACE ( 'NONE', ( #3026 ), #9451, .T. ) ;
#400 = CARTESIAN_POINT ( 'NONE',  ( -4.173491630687863108, -2.231261971483782691, 13.73605171672202019 ) ) ;
#401 = CARTESIAN_POINT ( 'NONE',  ( 1.229367062500000163, -13.00000000000000533, 0.1562499993172034307 ) ) ;
#402 = ORIENTED_EDGE ( 'NONE', *, *, #10343, .F. ) ;
#403 = CARTESIAN_POINT ( 'NONE',  ( 0.000000000000000000, 0.000000000000000000, 0.000000000000000000 ) ) ;
#404 = ORIENTED_EDGE ( 'NONE', *, *, #8112, .F. ) ;
#405 = PRESENTATION_LAYER_ASSIGNMENT (  '', '', ( #7352 ) ) ;
#406 = DIRECTION ( 'NONE',  ( 1.000000000000000000, 0.000000000000000000, 0.000000000000000000 ) ) ;
#407 = LINE ( 'NONE', #6055, #6780 ) ;
#408 = CARTESIAN_POINT ( 'NONE',  ( 10.00000000000000000, 6.100541242131515496, -3.528937025535514138 ) ) ;
#409 = VERTEX_POINT ( 'NONE', #6198 ) ;
#410 = CARTESIAN_POINT ( 'NONE',  ( -3.826313983664925811, -3.951860609387098489, 2.396051716722022551 ) ) ;
#411 = CARTESIAN_POINT ( 'NONE',  ( 2.625446233515515537, 5.152728359536502545, 11.05999999999999872 ) ) ;
#412 = CARTESIAN_POINT ( 'NONE',  ( -0.9046671180729963790, 5.711843387010016926, 7.979999999999999538 ) ) ;
#413 = ORIENTED_EDGE ( 'NONE', *, *, #3949, .T. ) ;
#414 = EDGE_CURVE ( 'NONE', #9650, #2266, #7804, .T. ) ;
#415 =( BOUNDED_CURVE ( )  B_SPLINE_CURVE ( 2, ( #2838, #7109, #4670, #2788, #2741, #9258, #6005 ),
 .UNSPECIFIED., .F., .T. ) 
 B_SPLINE_CURVE_WITH_KNOTS ( ( 3, 2, 2, 3 ),
 ( 0.7500000000000000000, 0.7777777777777777901, 0.8055555555555554692, 0.8333333333333332593 ),
 .UNSPECIFIED. ) 
 CURVE ( )  GEOMETRIC_REPRESENTATION_ITEM ( )  RATIONAL_B_SPLINE_CURVE ( ( 1.000000000000000000, 0.8660254037844387076, 1.000000000000000000, 0.8660254037844387076, 1.000000000000000000, 0.8660254037844392627, 0.9999999999999994449 ) ) 
 REPRESENTATION_ITEM ( '' )  );
#416 = CARTESIAN_POINT ( 'NONE',  ( -1.500000000000000222, -13.00000000000000533, -1.312500001365593416 ) ) ;
#417 = VECTOR ( 'NONE', #1476, 1000.000000000000000 ) ;
#418 = ORIENTED_EDGE ( 'NONE', *, *, #480, .T. ) ;
#419 = DIRECTION ( 'NONE',  ( 0.000000000000000000, -1.000000000000000000, 0.000000000000000000 ) ) ;
#420 = CARTESIAN_POINT ( 'NONE',  ( 3.535533905932731980, 3.535533905932744414, 13.99999999999999822 ) ) ;
#421 = ORIENTED_EDGE ( 'NONE', *, *, #5238, .T. ) ;
#422 = DIRECTION ( 'NONE',  ( 0.000000000000000000, -2.602085213965211430E-15, -1.000000000000000000 ) ) ;
#423 = DIRECTION ( 'NONE',  ( 0.000000000000000000, 0.000000000000000000, 1.000000000000000000 ) ) ;
#424 = CARTESIAN_POINT ( 'NONE',  ( 24.68830583033274806, -7.750000000000000000, 0.000000000000000000 ) ) ;
#425 = CARTESIAN_POINT ( 'NONE',  ( 1.963858260114715870, -4.049832306626327316, 11.04394828327797562 ) ) ;
#426 = ORIENTED_EDGE ( 'NONE', *, *, #10066, .T. ) ;
#427 = EDGE_CURVE ( 'NONE', #9096, #1645, #4210, .T. ) ;
#428 = AXIS2_PLACEMENT_3D ( 'NONE', #1380, #3660, #8440 ) ;
#429 = DIRECTION ( 'NONE',  ( 0.000000000000000000, 0.000000000000000000, 1.000000000000000000 ) ) ;
#430 = CARTESIAN_POINT ( 'NONE',  ( 8.000000000000001776, 6.100541242131515496, 3.528937025535514138 ) ) ;
#431 = CLOSED_SHELL ( 'NONE', ( #277, #9320, #9927, #8544, #10006, #399, #1911, #4446, #4671, #3762, #3426, #6874, #8625, #5452, #9045, #8690, #8125, #8773, #8910, #5128, #6954, #10114, #5058, #2205, #9564, #9977, #1593, #7544, #2557, #5719, #3320, #1896, #7278, #3681, #8319, #8899, #7533, #8941, #656, #771, #3259, #5912, #5057, #6064, #1527, #3579, #3527, #6993, #3388, #6405, #6791, #4611, #9290, #4035, #3186, #8628, #7763, #9179, #6201, #2777, #9603, #9417, #4009, #8640, #7128, #6228, #7169, #7521, #2767, #3637, #9890, #5832, #6553, #19, #1886, #7903, #7446, #7575 ) ) ;
#432 = FACE_OUTER_BOUND ( 'NONE', #1916, .T. ) ;
#433 = LINE ( 'NONE', #9391, #1094 ) ;
#434 = VECTOR ( 'NONE', #3012, 1000.000000000000000 ) ;
#435 = DIRECTION ( 'NONE',  ( 0.000000000000000000, 0.000000000000000000, 1.000000000000000000 ) ) ;
#436 = CARTESIAN_POINT ( 'NONE',  ( 0.000000000000000000, 0.000000000000000000, 0.000000000000000000 ) ) ;
#437 = FACE_OUTER_BOUND ( 'NONE', #3682, .T. ) ;
#438 = CARTESIAN_POINT ( 'NONE',  ( 3.411736077305382420, -3.279728542977940364, 12.89605171672202211 ) ) ;
#439 = CARTESIAN_POINT ( 'NONE',  ( 1.229367062500000385, -12.29022459553277002, -1.677083334016129967 ) ) ;
#440 = CARTESIAN_POINT ( 'NONE',  ( -5.697241258616385196, 0.9968613283357647958, 0.8239482832779764232 ) ) ;
#441 = PLANE ( 'NONE',  #10403 ) ;
#442 = CONICAL_SURFACE ( 'NONE', #7548, 1.249999999999997558, 1.029744258676650981 ) ;
#443 = ORIENTED_EDGE ( 'NONE', *, *, #1753, .F. ) ;
#444 = CARTESIAN_POINT ( 'NONE',  ( 1.300000000000000044, -1.478016689125442706, 1.843143693225357538E-15 ) ) ;
#445 = CARTESIAN_POINT ( 'NONE',  ( 25.00000000000000000, -4.000000000000000000, -2.000000000000000000 ) ) ;
#446 = DIRECTION ( 'NONE',  ( 0.000000000000000000, 0.000000000000000000, 1.000000000000000000 ) ) ;
#447 = EDGE_CURVE ( 'NONE', #6622, #1459, #1384, .T. ) ;
#448 = CARTESIAN_POINT ( 'NONE',  ( 1.300000000000000044, 1.478016689125442484, -1.626303258728256651E-15 ) ) ;
#449 = ORIENTED_EDGE ( 'NONE', *, *, #6016, .F. ) ;
#450 = CARTESIAN_POINT ( 'NONE',  ( -2.148092372876330813, -4.215868657802594122, 9.659999999999996589 ) ) ;
#451 = CARTESIAN_POINT ( 'NONE',  ( -0.7039550926810301812, -4.444597532678121965, 6.719999999999999751 ) ) ;
#452 = CARTESIAN_POINT ( 'NONE',  ( 0.7500000000000003331, -11.70096189432334732, -2.916666666666666963 ) ) ;
#453 = ORIENTED_EDGE ( 'NONE', *, *, #3517, .T. ) ;
#454 = ORIENTED_EDGE ( 'NONE', *, *, #1956, .T. ) ;
#455 = DIRECTION ( 'NONE',  ( 1.000000000000000000, 0.000000000000000000, 0.000000000000000000 ) ) ;
#456 = LINE ( 'NONE', #10272, #519 ) ;
#457 = EDGE_CURVE ( 'NONE', #3542, #5749, #6891, .T. ) ;
#458 = CARTESIAN_POINT ( 'NONE',  ( -2.000000000000000000, 4.438567988583180579, -7.249076783337634389 ) ) ;
#459 = ORIENTED_EDGE ( 'NONE', *, *, #8953, .F. ) ;
#460 = CARTESIAN_POINT ( 'NONE',  ( 2.542276634908080535, 5.195105386651229118, 9.256051716722023315 ) ) ;
#461 = CARTESIAN_POINT ( 'NONE',  ( -0.8603895577212598011, -5.432285873273260179, 9.519999999999999574 ) ) ;
#462 = CARTESIAN_POINT ( 'NONE',  ( 5.152728359536493663, 2.625446233515533745, 11.33999999999999808 ) ) ;
#463 = ORIENTED_EDGE ( 'NONE', *, *, #6523, .F. ) ;
#464 = CARTESIAN_POINT ( 'NONE',  ( -2.000000000000000000, 6.704570150427012543, -2.172265885002586661 ) ) ;
#465 = UNCERTAINTY_MEASURE_WITH_UNIT (LENGTH_MEASURE( 1.000000000000000082E-05 ), #9812, 'distance_accuracy_value', 'NONE');
#466 = SHAPE_REPRESENTATION_RELATIONSHIP ( 'NONE' , 'NONE' ,  #1027, #2591 ) ;
#467 = VERTEX_POINT ( 'NONE', #7099 ) ;
#468 = EDGE_CURVE ( 'NONE', #1004, #5848, #10298, .T. ) ;
#469 = CARTESIAN_POINT ( 'NONE',  ( 14.44459485323380754, -10.00000000000000000, -12.00000000000000000 ) ) ;
#470 = EDGE_CURVE ( 'NONE', #6865, #935, #9468, .T. ) ;
#471 = FACE_OUTER_BOUND ( 'NONE', #5653, .T. ) ;
#472 = EDGE_LOOP ( 'NONE', ( #8048, #6430, #5016, #6491 ) ) ;
#473 = DIRECTION ( 'NONE',  ( 0.000000000000000000, 0.000000000000000000, 1.000000000000000000 ) ) ;
#474 = DIRECTION ( 'NONE',  ( 0.000000000000000000, 0.000000000000000000, -1.000000000000000000 ) ) ;
#475 = CARTESIAN_POINT ( 'NONE',  ( -0.7916369971161423269, -4.430710083317576320, 11.32394828327797676 ) ) ;
#476 = ORIENTED_EDGE ( 'NONE', *, *, #8711, .T. ) ;
#477 = CARTESIAN_POINT ( 'NONE',  ( 0.000000000000000000, 52.93638525830372998, 2.343061888689529582 ) ) ;
#478 = CARTESIAN_POINT ( 'NONE',  ( -3.889087296526005044, -3.889087296526019255, 9.799999999999998934 ) ) ;
#479 = LINE ( 'NONE', #8439, #7690 ) ;
#480 = EDGE_CURVE ( 'NONE', #4172, #5208, #324, .T. ) ;
#481 = CARTESIAN_POINT ( 'NONE',  ( 24.68830583033274806, -7.750000000000000000, -12.00000000000000000 ) ) ;
#482 = CARTESIAN_POINT ( 'NONE',  ( 8.000000000000001776, -5.979767908488829775, -1.814490771706245065 ) ) ;
#483 = LINE ( 'NONE', #7749, #4325 ) ;
#484 = LINE ( 'NONE', #6725, #1123 ) ;
#485 = DIRECTION ( 'NONE',  ( 0.000000000000000000, 1.000000000000000000, 0.000000000000000000 ) ) ;
#486 = CARTESIAN_POINT ( 'NONE',  ( -3.345732310141667831, 3.345732310141653620, 2.099999999999999201 ) ) ;
#487 = CARTESIAN_POINT ( 'NONE',  ( -2.607672531582950546E-16, -14.41955080893447416, -1.968750000682796708 ) ) ;
#488 = CARTESIAN_POINT ( 'NONE',  ( -0.9480714621563718358, -5.418398423912716311, 0.1239482832779766203 ) ) ;
#489 = CARTESIAN_POINT ( 'NONE',  ( 8.692241771943170539E-17, -11.58044919106553650, -1.593750000682796708 ) ) ;
#490 = ORIENTED_EDGE ( 'NONE', *, *, #297, .F. ) ;
#491 = LINE ( 'NONE', #2876, #2720 ) ;
#492 = AXIS2_PLACEMENT_3D ( 'NONE', #2926, #2979, #637 ) ;
#493 = DIRECTION ( 'NONE',  ( 0.9396926207859105373, -0.3420201433256627732, 0.000000000000000000 ) ) ;
#494 = CARTESIAN_POINT ( 'NONE',  ( 3.000000000000000888, 0.000000000000000000, 0.000000000000000000 ) ) ;
#495 = DIRECTION ( 'NONE',  ( 0.000000000000000000, -0.5000000000000013323, -0.8660254037844378194 ) ) ;
#496 = PRODUCT_DEFINITION ( 'UNKNOWN', '', #10431, #818 ) ;
#497 = ORIENTED_EDGE ( 'NONE', *, *, #4647, .F. ) ;
#498 = CARTESIAN_POINT ( 'NONE',  ( 0.7401821875142697849, -4.673326407553650697, 3.779999999999998472 ) ) ;
#499 = CARTESIAN_POINT ( 'NONE',  ( -1.229367062500000385, -13.70977540446723886, -1.552083334016130189 ) ) ;
#500 = EDGE_LOOP ( 'NONE', ( #2992, #7233 ) ) ;
#501 = ORIENTED_EDGE ( 'NONE', *, *, #2913, .F. ) ;
#502 = DIRECTION ( 'NONE',  ( 0.000000000000000000, 0.000000000000000000, 1.000000000000000000 ) ) ;
#503 = AXIS2_PLACEMENT_3D ( 'NONE', #6182, #6020, #7784 ) ;
#504 = CARTESIAN_POINT ( 'NONE',  ( 20.72778015323380885, -10.00000000000000000, -12.00000000000000000 ) ) ;
#505 = VERTEX_POINT ( 'NONE', #7751 ) ;
#506 = CARTESIAN_POINT ( 'NONE',  ( 0.7727076532861471003, 5.446173322633805824, 6.316051716722022924 ) ) ;
#507 = LINE ( 'NONE', #562, #3552 ) ;
#508 = ORIENTED_EDGE ( 'NONE', *, *, #573, .F. ) ;
#509 = CARTESIAN_POINT ( 'NONE',  ( 23.26376179071655770, -10.02539999999999942, -12.00000000000000000 ) ) ;
#510 = CIRCLE ( 'NONE', #10175, 0.1499999999999999667 ) ;
#511 = ADVANCED_FACE ( 'NONE', ( #10357 ), #2867, .T. ) ;
#512 = ORIENTED_EDGE ( 'NONE', *, *, #4233, .T. ) ;
#513 = FILL_AREA_STYLE ('',( #1309 ) ) ;
#514 = AXIS2_PLACEMENT_3D ( 'NONE', #1323, #4706, #9556 ) ;
#515 = ORIENTED_EDGE ( 'NONE', *, *, #3261, .T. ) ;
#516 = AXIS2_PLACEMENT_3D ( 'NONE', #386, #236, #2717 ) ;
#517 = CARTESIAN_POINT ( 'NONE',  ( 1.499999999999999778, -13.86602540378444637, -2.541666666666666963 ) ) ;
#518 = LINE ( 'NONE', #5183, #846 ) ;
#519 = VECTOR ( 'NONE', #4424, 1000.000000000000000 ) ;
#520 = VERTEX_POINT ( 'NONE', #5255 ) ;
#521 = LINE ( 'NONE', #3697, #2869 ) ;
#522 = VECTOR ( 'NONE', #7006, 1000.000000000000000 ) ;
#523 = FACE_OUTER_BOUND ( 'NONE', #2494, .T. ) ;
#524 = CARTESIAN_POINT ( 'NONE',  ( 2.417848759854264618, -4.940838830814695548, 5.443948283277975975 ) ) ;
#525 = VERTEX_POINT ( 'NONE', #8496 ) ;
#526 = DIRECTION ( 'NONE',  ( 1.000000000000000000, 0.000000000000000000, 0.000000000000000000 ) ) ;
#527 = APPLICATION_CONTEXT ( 'automotive_design' ) ;
#528 = VECTOR ( 'NONE', #619, 1000.000000000000000 ) ;
#529 = EDGE_CURVE ( 'NONE', #5739, #8939, #8617, .T. ) ;
#530 = ADVANCED_FACE ( 'NONE', ( #437 ), #3663, .F. ) ;
#531 = CARTESIAN_POINT ( 'NONE',  ( 1.229367062500000163, -13.00000000000000533, -2.718750000682796486 ) ) ;
#532 = AXIS2_PLACEMENT_3D ( 'NONE', #7551, #3468, #3418 ) ;
#533 = SURFACE_SIDE_STYLE ('',( #7795 ) ) ;
#534 = CARTESIAN_POINT ( 'NONE',  ( -1.500000000000000666, -13.86602540378444637, -0.2083333333333333703 ) ) ;
#535 = DIRECTION ( 'NONE',  ( 0.3420201433256627732, -0.9396926207859105373, 0.000000000000000000 ) ) ;
#536 = DIRECTION ( 'NONE',  ( 1.000000000000000000, 0.000000000000000000, 0.000000000000000000 ) ) ;
#537 = DIRECTION ( 'NONE',  ( 0.000000000000000000, 0.000000000000000000, -1.000000000000000000 ) ) ;
#538 = CARTESIAN_POINT ( 'NONE',  ( 12.75489823682933554, -14.64240329930025375, 0.000000000000000000 ) ) ;
#539 = CARTESIAN_POINT ( 'NONE',  ( -2.122056237541221968, 3.969226411068977889, 11.63605171672202232 ) ) ;
#540 = CARTESIAN_POINT ( 'NONE',  ( 1.229367062500000385, -12.29022459553277002, -1.802083334016129967 ) ) ;
#541 = EDGE_CURVE ( 'NONE', #3837, #9529, #1280, .T. ) ;
#542 = CARTESIAN_POINT ( 'NONE',  ( -0.9480714621563718358, -5.418398423912716311, 11.32394828327797676 ) ) ;
#543 = CARTESIAN_POINT ( 'NONE',  ( -1.229367062500000163, -12.29022459553277002, -1.010416667349463227 ) ) ;
#544 = ORIENTED_EDGE ( 'NONE', *, *, #10139, .T. ) ;
#545 = CARTESIAN_POINT ( 'NONE',  ( 25.57717656966725883, 3.750000000000000000, 0.000000000000000000 ) ) ;
#546 = LINE ( 'NONE', #4618, #6946 ) ;
#547 = PLANE ( 'NONE',  #4834 ) ;
#548 = DIRECTION ( 'NONE',  ( 0.000000000000000000, -1.000000000000000000, -0.000000000000000000 ) ) ;
#549 = ORIENTED_EDGE ( 'NONE', *, *, #5107, .F. ) ;
#550 = DIRECTION ( 'NONE',  ( -1.000000000000000000, 0.000000000000000000, -0.000000000000000000 ) ) ;
#551 = DIRECTION ( 'NONE',  ( 1.000000000000000000, -0.000000000000000000, -0.000000000000000000 ) ) ;
#552 = EDGE_CURVE ( 'NONE', #7942, #3477, #1651, .T. ) ;
#553 = CARTESIAN_POINT ( 'NONE',  ( -3.411736077305382420, 3.279728542977939476, 14.29605171672202424 ) ) ;
#554 = CARTESIAN_POINT ( 'NONE',  ( -0.6146835312500006365, -14.06466310670085562, -1.010416667349463227 ) ) ;
#555 = ORIENTED_EDGE ( 'NONE', *, *, #4207, .T. ) ;
#556 = ORIENTED_EDGE ( 'NONE', *, *, #8304, .F. ) ;
#557 = CARTESIAN_POINT ( 'NONE',  ( 11.00000000000000355, 0.000000000000000000, 1.219500000000000028 ) ) ;
#558 = AXIS2_PLACEMENT_3D ( 'NONE', #2527, #5797, #5015 ) ;
#559 = CARTESIAN_POINT ( 'NONE',  ( 50.00005079999999680, 0.000000000000000000, 2.000000000000000000 ) ) ;
#560 = ORIENTED_EDGE ( 'NONE', *, *, #5898, .F. ) ;
#561 = CARTESIAN_POINT ( 'NONE',  ( 5.726445515403654873, -0.8124729078101852187, 12.61605171672202097 ) ) ;
#562 = CARTESIAN_POINT ( 'NONE',  ( 0.000000000000000000, -4.000000000000000000, -12.00000000000000000 ) ) ;
#563 = ORIENTED_EDGE ( 'NONE', *, *, #23, .F. ) ;
#564 = CARTESIAN_POINT ( 'NONE',  ( 1.500000000000000222, -12.13397459621556784, -1.458333333333333481 ) ) ;
#565 = EDGE_LOOP ( 'NONE', ( #3549, #2681, #8103, #9350 ) ) ;
#566 = AXIS2_PLACEMENT_3D ( 'NONE', #5875, #9125, #9777 ) ;
#567 = EDGE_CURVE ( 'NONE', #10377, #9650, #8751, .T. ) ;
#568 = ORIENTED_EDGE ( 'NONE', *, *, #8763, .F. ) ;
#569 = FACE_OUTER_BOUND ( 'NONE', #4760, .T. ) ;
#570 = LINE ( 'NONE', #3276, #6753 ) ;
#571 = ORIENTED_EDGE ( 'NONE', *, *, #4996, .F. ) ;
#572 = LINE ( 'NONE', #4540, #9658 ) ;
#573 = EDGE_CURVE ( 'NONE', #4283, #2644, #1679, .T. ) ;
#574 = CARTESIAN_POINT ( 'NONE',  ( 6.727620669667255804, -7.750000000000000000, -12.00000000000000000 ) ) ;
#575 = CARTESIAN_POINT ( 'NONE',  ( -0.9480714621563718358, -5.418398423912716311, 0.1239482832779766203 ) ) ;
#577 = ORIENTED_EDGE ( 'NONE', *, *, #6674, .F. ) ;
#576 = CIRCLE ( 'NONE', #8201, 2.000000000000001776 ) ;
#578 = CARTESIAN_POINT ( 'NONE',  ( 16.15239861966725599, 3.750000000000000000, 0.000000000000000000 ) ) ;
#579 = FACE_OUTER_BOUND ( 'NONE', #5973, .T. ) ;
#580 = PLANE ( 'NONE',  #2780 ) ;
#581 =( GEOMETRIC_REPRESENTATION_CONTEXT ( 3 ) GLOBAL_UNCERTAINTY_ASSIGNED_CONTEXT ( ( #4844 ) ) GLOBAL_UNIT_ASSIGNED_CONTEXT ( ( #7026, #8784, #10332 ) ) REPRESENTATION_CONTEXT ( 'NONE', 'WORKASPACE' ) );
#582 = DIRECTION ( 'NONE',  ( 1.000000000000000000, 0.000000000000000000, 0.000000000000000000 ) ) ;
#583 = CYLINDRICAL_SURFACE ( 'NONE', #1539, 2.750000000000000000 ) ;
#584 = LINE ( 'NONE', #9284, #1451 ) ;
#585 = CARTESIAN_POINT ( 'NONE',  ( 30.00000000000001066, -31.99999999999998579, 9.000000000000000000 ) ) ;
#586 = CARTESIAN_POINT ( 'NONE',  ( 5.999999999999999112, -27.00000000000000711, 3.000000000000000000 ) ) ;
#587 = CARTESIAN_POINT ( 'NONE',  ( -3.181980515339458027, -3.181980515339470905, 6.999999999999999112 ) ) ;
#588 = CARTESIAN_POINT ( 'NONE',  ( -2.607672531582950546E-16, -14.41955080893447416, -2.468750000682796486 ) ) ;
#589 = ORIENTED_EDGE ( 'NONE', *, *, #10211, .F. ) ;
#590 = CARTESIAN_POINT ( 'NONE',  ( -0.8124729078102072011, 5.726445515403652209, 12.58394828327797477 ) ) ;
#591 = CARTESIAN_POINT ( 'NONE',  ( 10.00000000000000000, 6.745408891279613961, -5.171987904998036178 ) ) ;
#592 = CIRCLE ( 'NONE', #5335, 1.280000000000000027 ) ;
#593 = EDGE_LOOP ( 'NONE', ( #8949, #9485, #3178, #7480 ) ) ;
#594 = LINE ( 'NONE', #3827, #4076 ) ;
#595 = EDGE_CURVE ( 'NONE', #8537, #2545, #5893, .T. ) ;
#596 = CARTESIAN_POINT ( 'NONE',  ( 25.00000000000000000, -4.000000000000000000, 0.000000000000000000 ) ) ;
#597 = LINE ( 'NONE', #648, #8239 ) ;
#598 = EDGE_CURVE ( 'NONE', #2046, #5731, #3289, .T. ) ;
#599 = CARTESIAN_POINT ( 'NONE',  ( 4.414205890716556446, 6.025400000000000311, -12.00000000000000000 ) ) ;
#600 = ORIENTED_EDGE ( 'NONE', *, *, #5420, .T. ) ;
#601 = CIRCLE ( 'NONE', #6521, 3.000000000000000000 ) ;
#602 = LINE ( 'NONE', #4677, #9302 ) ;
#603 = DIRECTION ( 'NONE',  ( 0.000000000000000000, -0.8660254037844391517, -0.4999999999999992784 ) ) ;
#604 = VECTOR ( 'NONE', #3880, 1000.000000000000000 ) ;
#605 = CARTESIAN_POINT ( 'NONE',  ( 0.7039550926810297371, 4.444597532678122853, 8.119999999999999218 ) ) ;
#606 = CARTESIAN_POINT ( 'NONE',  ( -0.7500000000000007772, -14.29903810567666156, -1.666666666666666741 ) ) ;
#607 = EDGE_LOOP ( 'NONE', ( #3342, #10479, #6748, #9581 ) ) ;
#608 = AXIS2_PLACEMENT_3D ( 'NONE', #7258, #8118, #4082 ) ;
#609 = ORIENTED_EDGE ( 'NONE', *, *, #2076, .T. ) ;
#610 = EDGE_CURVE ( 'NONE', #9996, #6690, #3028, .T. ) ;
#611 = CIRCLE ( 'NONE', #6015, 6.248999999999999666 ) ;
#612 = DIRECTION ( 'NONE',  ( 1.000000000000000000, 0.000000000000000000, 0.000000000000000000 ) ) ;
#613 = CARTESIAN_POINT ( 'NONE',  ( 0.000000000000000000, -4.000000000000000000, -12.00000000000000000 ) ) ;
#614 = VERTEX_POINT ( 'NONE', #9666 ) ;
#615 = CARTESIAN_POINT ( 'NONE',  ( -5.110351332421769754, -2.708615832122969191, 10.93605171672202125 ) ) ;
#616 = LINE ( 'NONE', #5484, #9988 ) ;
#617 = DIRECTION ( 'NONE',  ( -0.000000000000000000, -0.000000000000000000, 1.000000000000000000 ) ) ;
#618 = VERTEX_POINT ( 'NONE', #10411 ) ;
#619 = DIRECTION ( 'NONE',  ( 1.000000000000000000, -0.000000000000000000, -0.000000000000000000 ) ) ;
#620 = CARTESIAN_POINT ( 'NONE',  ( -0.7727076532861475444, -5.446173322633804048, 10.51605171672202133 ) ) ;
#621 = ORIENTED_EDGE ( 'NONE', *, *, #4647, .T. ) ;
#622 = ORIENTED_EDGE ( 'NONE', *, *, #4233, .F. ) ;
#623 = DIRECTION ( 'NONE',  ( -1.000000000000000000, -0.000000000000000000, -0.000000000000000000 ) ) ;
#624 = DIRECTION ( 'NONE',  ( 0.9396926207859105373, 0.3420201433256627732, 0.000000000000000000 ) ) ;
#625 = ORIENTED_EDGE ( 'NONE', *, *, #5895, .F. ) ;
#626 = CARTESIAN_POINT ( 'NONE',  ( -2.000000000000000000, 5.904264776415129923, -2.046865518294644914 ) ) ;
#627 = DIRECTION ( 'NONE',  ( 1.000000000000000000, 0.000000000000000000, 0.000000000000000000 ) ) ;
#628 = EDGE_CURVE ( 'NONE', #4280, #1390, #7154, .T. ) ;
#629 = CARTESIAN_POINT ( 'NONE',  ( 0.9480714621563713917, 5.418398423912717199, 7.123948283277974802 ) ) ;
#630 = ORIENTED_EDGE ( 'NONE', *, *, #598, .F. ) ;
#631 = DIRECTION ( 'NONE',  ( 1.000000000000000000, 0.000000000000000000, -0.000000000000000000 ) ) ;
#632 = DIRECTION ( 'NONE',  ( 0.000000000000000000, 0.000000000000000000, 1.000000000000000000 ) ) ;
#633 = CARTESIAN_POINT ( 'NONE',  ( 1.300000000000000044, 0.000000000000000000, 0.000000000000000000 ) ) ;
#634 = CARTESIAN_POINT ( 'NONE',  ( 0.000000000000000000, -10.00000000000000000, -12.00000000000000000 ) ) ;
#635 = DIRECTION ( 'NONE',  ( -0.000000000000000000, -0.000000000000000000, 1.000000000000000000 ) ) ;
#636 = FACE_BOUND ( 'NONE', #3921, .T. ) ;
#637 = DIRECTION ( 'NONE',  ( 0.000000000000000000, 0.000000000000000000, 1.000000000000000000 ) ) ;
#638 = CARTESIAN_POINT ( 'NONE',  ( 4.215868657802586128, 2.148092372876346801, 2.939999999999999059 ) ) ;
#639 = CARTESIAN_POINT ( 'NONE',  ( -1.229367062500000163, -13.00000000000000533, 0.03124999931720332663 ) ) ;
#640 = CARTESIAN_POINT ( 'NONE',  ( 2.708615832122949652, 5.110351332421781301, 12.86394828327797768 ) ) ;
#641 = CARTESIAN_POINT ( 'NONE',  ( 16.15239861966725599, -7.750000000000000000, -12.00000000000000000 ) ) ;
#642 = ADVANCED_FACE ( 'NONE', ( #9719 ), #6462, .T. ) ;
#643 = EDGE_LOOP ( 'NONE', ( #2365, #568, #1143, #6976 ) ) ;
#644 = SHAPE_DEFINITION_REPRESENTATION ( #7147, #9430 ) ;
#645 = CARTESIAN_POINT ( 'NONE',  ( 8.000000000000001776, 4.561279057474473930, -4.271385531633122845 ) ) ;
#646 = CARTESIAN_POINT ( 'NONE',  ( -2.000000000000000000, 7.008469740302810891, -0.7425307242147085596 ) ) ;
#647 = CARTESIAN_POINT ( 'NONE',  ( 1.500000000000000222, -13.00000000000000533, 0.4374999986344065284 ) ) ;
#648 = CARTESIAN_POINT ( 'NONE',  ( 1.999999999999986233, 15.00000000000000355, -4.000000000000009770 ) ) ;
#649 = DIRECTION ( 'NONE',  ( 0.3420201433256627732, 0.9396926207859105373, 0.000000000000000000 ) ) ;
#650 = ORIENTED_EDGE ( 'NONE', *, *, #2389, .T. ) ;
#651 = PRESENTATION_STYLE_ASSIGNMENT (( #2303 ) ) ;
#652 = DIRECTION ( 'NONE',  ( 0.000000000000000000, -1.154631945610162802E-14, -1.000000000000000000 ) ) ;
#653 = CARTESIAN_POINT ( 'NONE',  ( -4.009529358847660596, 2.042957248827953265, 13.15999999999999837 ) ) ;
#654 = EDGE_CURVE ( 'NONE', #729, #8371, #1490, .T. ) ;
#655 = CARTESIAN_POINT ( 'NONE',  ( 1.500000000000000222, -13.00000000000000533, -1.500000000000000000 ) ) ;
#656 = ADVANCED_FACE ( 'NONE', ( #4031 ), #3184, .F. ) ;
#657 = AXIS2_PLACEMENT_3D ( 'NONE', #1217, #8778, #8485 ) ;
#658 = EDGE_LOOP ( 'NONE', ( #8231, #8896, #2249, #3731 ) ) ;
#659 = ORIENTED_EDGE ( 'NONE', *, *, #7728, .T. ) ;
#660 = CARTESIAN_POINT ( 'NONE',  ( 25.00000000000000000, -7.750000000000000000, -12.00000000000000000 ) ) ;
#661 = DIRECTION ( 'NONE',  ( 0.000000000000000000, 0.000000000000000000, 1.000000000000000000 ) ) ;
#662 = ORIENTED_EDGE ( 'NONE', *, *, #2847, .T. ) ;
#663 = CARTESIAN_POINT ( 'NONE',  ( -2.576046737280769605, 4.860232935257343456, 11.63605171672202232 ) ) ;
#664 = STYLED_ITEM ( 'NONE', ( #651 ), #1029 ) ;
#665 = CARTESIAN_POINT ( 'NONE',  ( 0.000000000000000000, -13.00000000000000533, -3.000000000000000000 ) ) ;
#666 = DIRECTION ( 'NONE',  ( -1.000000000000000000, 0.000000000000000000, 0.000000000000000000 ) ) ;
#667 = ORIENTED_EDGE ( 'NONE', *, *, #7014, .F. ) ;
#668 = AXIS2_PLACEMENT_3D ( 'NONE', #5379, #617, #3899 ) ;
#669 = DIRECTION ( 'NONE',  ( 0.000000000000000000, 0.000000000000000000, 1.000000000000000000 ) ) ;
#670 = CARTESIAN_POINT ( 'NONE',  ( 4.687928535947288644, -0.6479879772514620662, 1.416051716722023235 ) ) ;
#671 = EDGE_CURVE ( 'NONE', #6869, #4944, #2339, .T. ) ;
#672 = AXIS2_PLACEMENT_3D ( 'NONE', #9186, #234, #7433 ) ;
#673 = ORIENTED_EDGE ( 'NONE', *, *, #10174, .F. ) ;
#674 = SURFACE_STYLE_FILL_AREA ( #513 ) ;
#675 = VECTOR ( 'NONE', #8846, 1000.000000000000000 ) ;
#676 = LINE ( 'NONE', #2269, #8398 ) ;
#677 = VECTOR ( 'NONE', #10171, 1000.000000000000000 ) ;
#678 = CARTESIAN_POINT ( 'NONE',  ( -5.999999999999999112, 26.99999999999999289, 3.000000000000000000 ) ) ;
#679 = ORIENTED_EDGE ( 'NONE', *, *, #5695, .T. ) ;
#680 = CARTESIAN_POINT ( 'NONE',  ( 21.54671318033274829, -7.750000000000000000, -12.00000000000000000 ) ) ;
#681 = DIRECTION ( 'NONE',  ( -1.156482317317871478E-16, 1.000000000000000000, 0.000000000000000000 ) ) ;
#682 = CARTESIAN_POINT ( 'NONE',  ( -2.417848759854264618, 4.940838830814694660, 4.043948283277976508 ) ) ;
#683 = ORIENTED_EDGE ( 'NONE', *, *, #7002, .F. ) ;
#684 = VECTOR ( 'NONE', #1145, 1000.000000000000000 ) ;
#685 = CARTESIAN_POINT ( 'NONE',  ( 0.7500000000000003331, -11.70096189432334732, 0.02083333196773980503 ) ) ;
#686 = CIRCLE ( 'NONE', #2043, 3.000000000000000888 ) ;
#687 = CARTESIAN_POINT ( 'NONE',  ( -1.500000000000000222, -13.00000000000000533, -0.3125000013655936937 ) ) ;
#688 = SURFACE_STYLE_USAGE ( .BOTH. , #533 ) ;
#689 = ADVANCED_BREP_SHAPE_REPRESENTATION ( '', ( #1029, #2101 ), #5648 ) ;
#690 = ORIENTED_EDGE ( 'NONE', *, *, #6660, .T. ) ;
#691 = AXIS2_PLACEMENT_3D ( 'NONE', #2203, #3948, #9582 ) ;
#692 = CARTESIAN_POINT ( 'NONE',  ( -2.000000000000015099, 35.00000000000000000, 3.999999999999986233 ) ) ;
#693 = AXIS2_PLACEMENT_3D ( 'NONE', #10001, #3572, #9409 ) ;
#694 = DIRECTION ( 'NONE',  ( 0.000000000000000000, 0.000000000000000000, 1.000000000000000000 ) ) ;
#695 = CARTESIAN_POINT ( 'NONE',  ( -2.000000000000000000, -2.652816298622379776, -5.657964889053610946 ) ) ;
#696 = DIRECTION ( 'NONE',  ( -1.000000000000000000, -2.312964634635742957E-16, 0.000000000000000000 ) ) ;
#697 = VECTOR ( 'NONE', #5045, 1000.000000000000114 ) ;
#698 = DIRECTION ( 'NONE',  ( -1.000000000000000000, -0.000000000000000000, -0.000000000000000000 ) ) ;
#699 = CARTESIAN_POINT ( 'NONE',  ( -4.215868657802586128, -2.148092372876348133, 7.139999999999997016 ) ) ;
#700 = CARTESIAN_POINT ( 'NONE',  ( 0.6146835312499993043, -14.06466310670085562, 0.1979166659838698661 ) ) ;
#701 = VECTOR ( 'NONE', #1350, 1000.000000000000000 ) ;
#702 = CARTESIAN_POINT ( 'NONE',  ( 3.951860609387084722, 3.826313983664940022, 7.403948283277976827 ) ) ;
#703 = LINE ( 'NONE', #3932, #906 ) ;
#704 = ORIENTED_EDGE ( 'NONE', *, *, #9980, .F. ) ;
#705 = EDGE_CURVE ( 'NONE', #1471, #10128, #9772, .T. ) ;
#706 = CARTESIAN_POINT ( 'NONE',  ( -2.625446233515515537, -5.152728359536502545, 1.259999999999999787 ) ) ;
#707 = DIRECTION ( 'NONE',  ( 0.000000000000000000, 0.000000000000000000, -1.000000000000000000 ) ) ;
#708 = EDGE_LOOP ( 'NONE', ( #5948, #2687, #4855, #10434, #9641, #7515, #7392, #3265, #7780, #4226, #690, #4016, #8469, #9796, #6235 ) ) ;
#709 = CARTESIAN_POINT ( 'NONE',  ( 4.000000000000000888, 8.265874651078044977, -1.981241088980697729 ) ) ;
#710 = LINE ( 'NONE', #7975, #863 ) ;
#711 = CARTESIAN_POINT ( 'NONE',  ( 0.000000000000000000, -10.00000000000000000, 0.000000000000000000 ) ) ;
#712 = EDGE_CURVE ( 'NONE', #980, #3093, #750, .T. ) ;
#713 = DIRECTION ( 'NONE',  ( 1.156482317317871478E-16, -1.000000000000000000, 0.000000000000000000 ) ) ;
#714 = CARTESIAN_POINT ( 'NONE',  ( -13.00000000000000000, 19.99999999999999645, -9.000000000000000000 ) ) ;
#715 = CARTESIAN_POINT ( 'NONE',  ( -4.215868657802586128, -2.148092372876348133, 12.73999999999999488 ) ) ;
#716 = CARTESIAN_POINT ( 'NONE',  ( 0.7500000000000003331, -11.70096189432334732, -0.9166666666666667407 ) ) ;
#717 = VERTEX_POINT ( 'NONE', #2500 ) ;
#718 = ORIENTED_EDGE ( 'NONE', *, *, #4535, .F. ) ;
#719 = CARTESIAN_POINT ( 'NONE',  ( 10.68814634676619590, -10.00000000000000000, -12.00000000000000000 ) ) ;
#720 = ORIENTED_EDGE ( 'NONE', *, *, #4047, .T. ) ;
#721 = EDGE_CURVE ( 'NONE', #3971, #3139, #8290, .T. ) ;
#722 = DIRECTION ( 'NONE',  ( -0.3420201433256627732, 0.9396926207859105373, 0.000000000000000000 ) ) ;
#723 = LINE ( 'NONE', #6220, #677 ) ;
#724 = ORIENTED_EDGE ( 'NONE', *, *, #8186, .F. ) ;
#725 = CARTESIAN_POINT ( 'NONE',  ( 0.000000000000000000, 0.000000000000000000, 0.000000000000000000 ) ) ;
#726 = CARTESIAN_POINT ( 'NONE',  ( -4.430710083317573655, -0.7916369971161599794, 2.676051716722023244 ) ) ;
#727 = ORIENTED_EDGE ( 'NONE', *, *, #1997, .F. ) ;
#728 = SURFACE_STYLE_USAGE ( .BOTH. , #9540 ) ;
#729 = VERTEX_POINT ( 'NONE', #10467 ) ;
#730 = AXIS2_PLACEMENT_3D ( 'NONE', #6023, #9492, #6879 ) ;
#731 = CARTESIAN_POINT ( 'NONE',  ( 0.000000000000000000, -4.000000000000000000, -10.00000000000000000 ) ) ;
#732 = DIRECTION ( 'NONE',  ( 0.000000000000000000, 0.000000000000000000, -1.000000000000000000 ) ) ;
#733 = ORIENTED_EDGE ( 'NONE', *, *, #2748, .F. ) ;
#734 = EDGE_CURVE ( 'NONE', #7181, #6113, #8913, .T. ) ;
#735 = CARTESIAN_POINT ( 'NONE',  ( 0.9046671180729951578, -5.711843387010016926, 6.579999999999999183 ) ) ;
#736 = ADVANCED_FACE ( 'NONE', ( #5713 ), #5223, .F. ) ;
#737 = DIRECTION ( 'NONE',  ( -1.000000000000000000, -0.000000000000000000, -0.000000000000000000 ) ) ;
#738 = CARTESIAN_POINT ( 'NONE',  ( -4.860232935257354114, 2.576046737280751842, 0.9639482832779766586 ) ) ;
#739 = ORIENTED_EDGE ( 'NONE', *, *, #9069, .T. ) ;
#740 = CARTESIAN_POINT ( 'NONE',  ( -0.7499999999999997780, -11.70096189432334555, -0.3958333346989269530 ) ) ;
#741 = CIRCLE ( 'NONE', #9725, 4.000000000000000000 ) ;
#742 = DIRECTION ( 'NONE',  ( 0.000000000000000000, -1.000000000000000000, -0.000000000000000000 ) ) ;
#743 = ORIENTED_EDGE ( 'NONE', *, *, #734, .F. ) ;
#744 = CARTESIAN_POINT ( 'NONE',  ( 0.4444353696672553311, -7.750000000000000000, -12.00000000000000000 ) ) ;
#745 = DIRECTION ( 'NONE',  ( 0.000000000000000000, 0.000000000000000000, -1.000000000000000000 ) ) ;
#746 = FACE_OUTER_BOUND ( 'NONE', #9469, .T. ) ;
#747 = VECTOR ( 'NONE', #5775, 1000.000000000000000 ) ;
#748 = EDGE_CURVE ( 'NONE', #10270, #6751, #4270, .T. ) ;
#749 = FACE_OUTER_BOUND ( 'NONE', #2071, .T. ) ;
#750 = LINE ( 'NONE', #3983, #6059 ) ;
#751 = CARTESIAN_POINT ( 'NONE',  ( 4.009529358847659708, -2.042957248827953709, 3.359999999999999876 ) ) ;
#752 = ORIENTED_EDGE ( 'NONE', *, *, #63, .T. ) ;
#753 = FACE_OUTER_BOUND ( 'NONE', #4033, .T. ) ;
#754 = CARTESIAN_POINT ( 'NONE',  ( -5.195105386651219348, -2.542276634908102295, 8.943948283277975975 ) ) ;
#755 = AXIS2_PLACEMENT_3D ( 'NONE', #9759, #8791, #4917 ) ;
#756 = DIRECTION ( 'NONE',  ( -1.000000000000000000, -0.000000000000000000, -0.000000000000000000 ) ) ;
#757 = ORIENTED_EDGE ( 'NONE', *, *, #23, .T. ) ;
#758 = DIRECTION ( 'NONE',  ( 0.000000000000000000, 0.000000000000000000, 1.000000000000000000 ) ) ;
#759 = DIRECTION ( 'NONE',  ( 0.000000000000000000, 0.000000000000000000, 1.000000000000000000 ) ) ;
#760 = ORIENTED_EDGE ( 'NONE', *, *, #6615, .F. ) ;
#761 = DIRECTION ( 'NONE',  ( 4.625929269271485914E-16, -1.000000000000000000, 0.000000000000000000 ) ) ;
#762 = CARTESIAN_POINT ( 'NONE',  ( 30.00000000000001066, 35.00000000000001421, 5.999999999999999112 ) ) ;
#763 = CARTESIAN_POINT ( 'NONE',  ( 1.300000000000000044, 1.478016689125442484, -1.626303258728256651E-15 ) ) ;
#764 = DIRECTION ( 'NONE',  ( 1.000000000000000000, 0.000000000000000000, 0.000000000000000000 ) ) ;
#765 = CYLINDRICAL_SURFACE ( 'NONE', #10346, 8.500000000000000000 ) ;
#766 = VECTOR ( 'NONE', #8542, 1000.000000000000000 ) ;
#767 = CARTESIAN_POINT ( 'NONE',  ( 1.963858260114715870, -4.049832306626327316, -0.1560517167220233370 ) ) ;
#768 = CARTESIAN_POINT ( 'NONE',  ( 1.060575238724907038E-16, -11.26794919243112680, -0.8750000000000004441 ) ) ;
#769 = PRESENTATION_LAYER_ASSIGNMENT (  '', '', ( #2794 ) ) ;
#770 = ORIENTED_EDGE ( 'NONE', *, *, #4732, .T. ) ;
#771 = ADVANCED_FACE ( 'NONE', ( #2069 ), #4745, .T. ) ;
#772 = ORIENTED_EDGE ( 'NONE', *, *, #3509, .F. ) ;
#773 = CARTESIAN_POINT ( 'NONE',  ( -2.000000000000000000, 2.871924938129970517, -6.435996203144478400 ) ) ;
#774 = CIRCLE ( 'NONE', #8227, 1.500000000000000222 ) ;
#775 = CARTESIAN_POINT ( 'NONE',  ( 1.500000000000000222, -12.13397459621556784, -2.520833334698926897 ) ) ;
#776 = ORIENTED_EDGE ( 'NONE', *, *, #9858, .T. ) ;
#777 = VECTOR ( 'NONE', #1134, 1000.000000000000000 ) ;
#778 = CARTESIAN_POINT ( 'NONE',  ( -29.99999999999998934, -35.00000000000000000, 9.000000000000000000 ) ) ;
#779 = ORIENTED_EDGE ( 'NONE', *, *, #1512, .F. ) ;
#780 = CARTESIAN_POINT ( 'NONE',  ( 2.064922774268895811, 4.258245684917319807, 3.656051716722022782 ) ) ;
#781 = VECTOR ( 'NONE', #5041, 1000.000000000000000 ) ;
#782 = ORIENTED_EDGE ( 'NONE', *, *, #6286, .F. ) ;
#783 = AXIS2_PLACEMENT_3D ( 'NONE', #9681, #8871, #7111 ) ;
#784 = EDGE_CURVE ( 'NONE', #614, #8730, #616, .T. ) ;
#785 = EDGE_LOOP ( 'NONE', ( #7570, #6158, #4302, #1621 ) ) ;
#786 = DIRECTION ( 'NONE',  ( 0.000000000000000000, -1.000000000000000000, 1.026972870230479989E-15 ) ) ;
#787 = EDGE_CURVE ( 'NONE', #8703, #2420, #2314, .T. ) ;
#788 = CARTESIAN_POINT ( 'NONE',  ( -1.499999999999998224, -12.13397459621556607, -1.791666666666667185 ) ) ;
#789 = VERTEX_POINT ( 'NONE', #424 ) ;
#790 = CARTESIAN_POINT ( 'NONE',  ( 4.900535883036028828, -2.496947748567499126, 8.959999999999999076 ) ) ;
#791 = LINE ( 'NONE', #6345, #391 ) ;
#792 = CARTESIAN_POINT ( 'NONE',  ( 4.023224611898322145, -4.155232146225737111, 10.90394828327797327 ) ) ;
#793 = ORIENTED_EDGE ( 'NONE', *, *, #10301, .T. ) ;
#794 = CARTESIAN_POINT ( 'NONE',  ( 1.500000000000000444, -12.13397459621556607, -0.5208333346989270085 ) ) ;
#795 = ADVANCED_FACE ( 'NONE', ( #7932 ), #3599, .T. ) ;
#796 = EDGE_CURVE ( 'NONE', #10128, #1894, #6384, .T. ) ;
#797 = ADVANCED_FACE ( 'NONE', ( #10440 ), #5240, .T. ) ;
#798 = VERTEX_POINT ( 'NONE', #4633 ) ;
#799 = LINE ( 'NONE', #5612, #2459 ) ;
#800 = CARTESIAN_POINT ( 'NONE',  ( 2.399999999999999911, 2.939152317953647106E-16, 6.999999999999999112 ) ) ;
#801 = LINE ( 'NONE', #3182, #7893 ) ;
#802 = CARTESIAN_POINT ( 'NONE',  ( 4.000000000000000888, -5.522688772756355391, -6.461416928141300531 ) ) ;
#803 = DIRECTION ( 'NONE',  ( 0.000000000000000000, 0.000000000000000000, 1.000000000000000000 ) ) ;
#804 = CARTESIAN_POINT ( 'NONE',  ( 4.258245684917310037, 2.064922774268912686, 1.943948283277976419 ) ) ;
#805 = EDGE_LOOP ( 'NONE', ( #3050, #7525, #1781, #3634 ) ) ;
#806 = CARTESIAN_POINT ( 'NONE',  ( -0.6146835312499998594, -11.93533689329915326, -0.6770833340161300784 ) ) ;
#807 = CARTESIAN_POINT ( 'NONE',  ( 2.496947748567516889, -4.900535883036019946, 3.639999999999999680 ) ) ;
#808 = EDGE_CURVE ( 'NONE', #505, #2310, #6880, .T. ) ;
#809 = DIRECTION ( 'NONE',  ( 0.000000000000000000, 0.000000000000000000, -1.000000000000000000 ) ) ;
#810 = CARTESIAN_POINT ( 'NONE',  ( 0.8603895577212593571, 5.432285873273261068, 2.519999999999999574 ) ) ;
#811 = DIRECTION ( 'NONE',  ( 1.000000000000000000, 0.000000000000000000, 0.000000000000000000 ) ) ;
#812 = CARTESIAN_POINT ( 'NONE',  ( 17.57694265928344635, 6.025400000000000311, -12.00000000000000000 ) ) ;
#813 = DIRECTION ( 'NONE',  ( -1.000000000000000000, -0.000000000000000000, -0.000000000000000000 ) ) ;
#814 = CARTESIAN_POINT ( 'NONE',  ( 7.555798540716556211, 6.025400000000000311, 0.000000000000000000 ) ) ;
#815 = CARTESIAN_POINT ( 'NONE',  ( 0.000000000000000000, -13.00000000000000533, 0.000000000000000000 ) ) ;
#816 = LINE ( 'NONE', #2514, #6764 ) ;
#817 = CARTESIAN_POINT ( 'NONE',  ( -0.7916369971161423269, -4.430710083317576320, 0.1239482832779766203 ) ) ;
#818 = PRODUCT_DEFINITION_CONTEXT ( 'detailed design', #5599, 'design' ) ;
#819 = CARTESIAN_POINT ( 'NONE',  ( -1.500000000000000000, -12.13397459621556607, -1.791666666666666741 ) ) ;
#820 = ORIENTED_EDGE ( 'NONE', *, *, #940, .F. ) ;
#821 = ORIENTED_EDGE ( 'NONE', *, *, #2159, .T. ) ;
#822 = CARTESIAN_POINT ( 'NONE',  ( 5.999999999999999112, -27.00000000000000711, 3.000000000000000000 ) ) ;
#823 = LINE ( 'NONE', #9950, #1369 ) ;
#824 = ORIENTED_EDGE ( 'NONE', *, *, #3871, .F. ) ;
#825 = CARTESIAN_POINT ( 'NONE',  ( 4.009529358847659708, -2.042957248827953709, 3.359999999999999876 ) ) ;
#826 = CARTESIAN_POINT ( 'NONE',  ( -2.000000000000000000, 4.058600654062950674, -7.468451026206158083 ) ) ;
#827 = ORIENTED_EDGE ( 'NONE', *, *, #925, .F. ) ;
#828 = EDGE_CURVE ( 'NONE', #5863, #2098, #3844, .T. ) ;
#829 = VECTOR ( 'NONE', #7182, 1000.000000000000227 ) ;
#830 = CARTESIAN_POINT ( 'NONE',  ( -0.9968613283357868893, 5.697241258616382531, 11.77605171672202289 ) ) ;
#831 = ORIENTED_EDGE ( 'NONE', *, *, #5642, .T. ) ;
#832 =( NAMED_UNIT ( * ) SI_UNIT ( $, .STERADIAN. ) SOLID_ANGLE_UNIT ( ) );
#833 = EDGE_LOOP ( 'NONE', ( #2518, #4015, #6107, #8146 ) ) ;
#834 = LINE ( 'NONE', #4066, #3644 ) ;
#835 = AXIS2_PLACEMENT_3D ( 'NONE', #8806, #698, #3239 ) ;
#836 = CARTESIAN_POINT ( 'NONE',  ( -2.000000000000000000, 52.93638525830372998, 2.343061888689529582 ) ) ;
#837 = VERTEX_POINT ( 'NONE', #2366 ) ;
#838 = AXIS2_PLACEMENT_3D ( 'NONE', #8631, #1368, #3801 ) ;
#839 = CARTESIAN_POINT ( 'NONE',  ( -4.089228379062038066, 4.089228379062021190, 7.699999999999998401 ) ) ;
#840 = CARTESIAN_POINT ( 'NONE',  ( 11.00000000000000355, 1.219500000000000028, 0.000000000000000000 ) ) ;
#841 = CARTESIAN_POINT ( 'NONE',  ( 2.417848759854264618, -4.940838830814695548, 11.04394828327797562 ) ) ;
#842 = ORIENTED_EDGE ( 'NONE', *, *, #902, .F. ) ;
#843 = CLOSED_SHELL ( 'NONE', ( #7151, #129, #1567, #8897, #9633, #4992, #3175, #8197, #2905, #8321, #2086, #3112, #8363, #5266, #10473, #8475, #5747, #9474, #6974, #1129, #4223, #6918, #511, #2544, #4107, #7035, #6532, #8445, #5830, #8827, #288, #5462, #6321, #1838, #7810, #4341, #5967, #9961, #9615, #5841, #3362, #795, #9948, #6931, #5514, #4220, #8577, #2099, #3356, #8417 ) ) ;
#844 = CARTESIAN_POINT ( 'NONE',  ( -1.500000000000000666, -13.86602540378444459, -0.2708333346989268420 ) ) ;
#845 = EDGE_CURVE ( 'NONE', #1584, #1356, #4688, .T. ) ;
#846 = VECTOR ( 'NONE', #2165, 1000.000000000000000 ) ;
#847 = VECTOR ( 'NONE', #349, 1000.000000000000000 ) ;
#848 = ORIENTED_EDGE ( 'NONE', *, *, #9343, .F. ) ;
#849 = CARTESIAN_POINT ( 'NONE',  ( -1.500000000000000222, -13.00000000000000533, -0.8125000013655935271 ) ) ;
#850 = FACE_OUTER_BOUND ( 'NONE', #7920, .T. ) ;
#851 = DIRECTION ( 'NONE',  ( 1.000000000000000000, 0.000000000000000000, -0.000000000000000000 ) ) ;
#852 = FACE_OUTER_BOUND ( 'NONE', #4523, .T. ) ;
#853 = CIRCLE ( 'NONE', #3726, 2.600000000000000089 ) ;
#854 = DIRECTION ( 'NONE',  ( -0.000000000000000000, -1.000000000000000000, -0.000000000000000000 ) ) ;
#855 = CARTESIAN_POINT ( 'NONE',  ( 3.969226411068985882, -2.122056237541205981, 5.163948283277975726 ) ) ;
#856 = ADVANCED_FACE ( 'NONE', ( #9639 ), #6825, .F. ) ;
#857 = ORIENTED_EDGE ( 'NONE', *, *, #902, .T. ) ;
#858 = VECTOR ( 'NONE', #1332, 1000.000000000000000 ) ;
#859 = EDGE_CURVE ( 'NONE', #6218, #8785, #9534, .T. ) ;
#860 = CARTESIAN_POINT ( 'NONE',  ( -2.607672531582950546E-16, -14.41955080893447416, -0.9687500006827967081 ) ) ;
#861 = CARTESIAN_POINT ( 'NONE',  ( 5.711843387010018702, -0.9046671180729751738, 8.820000000000000284 ) ) ;
#862 = DIRECTION ( 'NONE',  ( 1.000000000000000000, 0.000000000000000000, 0.000000000000000000 ) ) ;
#863 = VECTOR ( 'NONE', #8661, 1000.000000000000000 ) ;
#864 = CONTEXT_DEPENDENT_SHAPE_REPRESENTATION ( #1817, #9555 ) ;
#865 = VECTOR ( 'NONE', #4833, 1000.000000000000000 ) ;
#866 = CARTESIAN_POINT ( 'NONE',  ( 22.43558391966725907, 3.750000000000000000, 0.000000000000000000 ) ) ;
#867 = CIRCLE ( 'NONE', #2217, 1.999999999999997780 ) ;
#868 = DIRECTION ( 'NONE',  ( 0.000000000000000000, 0.4999999999999991673, -0.8660254037844391517 ) ) ;
#869 = CARTESIAN_POINT ( 'NONE',  ( -2.000000000000000000, 6.100541242131515496, 3.528937025535514138 ) ) ;
#870 = CYLINDRICAL_SURFACE ( 'NONE', #6948, 1.599999999999998979 ) ;
#871 = AXIS2_PLACEMENT_3D ( 'NONE', #3735, #4797, #7928 ) ;
#872 = LINE ( 'NONE', #1720, #1339 ) ;
#873 = CARTESIAN_POINT ( 'NONE',  ( 4.430710083317573655, 0.7916369971161595354, 6.876051716722023421 ) ) ;
#874 = EDGE_CURVE ( 'NONE', #6381, #8915, #7129, .T. ) ;
#875 = CARTESIAN_POINT ( 'NONE',  ( -2.499999999999992895, -31.99999999999999289, 3.061616997868383141E-16 ) ) ;
#876 = LINE ( 'NONE', #8034, #6940 ) ;
#877 = CARTESIAN_POINT ( 'NONE',  ( -3.969226411068985882, 2.122056237541205537, 6.563948283277975193 ) ) ;
#878 = VECTOR ( 'NONE', #10387, 1000.000000000000000 ) ;
#879 = CARTESIAN_POINT ( 'NONE',  ( -0.6146835312499998594, -11.93533689329915326, -2.552083334016129967 ) ) ;
#880 = ORIENTED_EDGE ( 'NONE', *, *, #4483, .T. ) ;
#881 = ORIENTED_EDGE ( 'NONE', *, *, #2871, .T. ) ;
#882 = DIRECTION ( 'NONE',  ( 0.000000000000000000, 0.000000000000000000, -1.000000000000000000 ) ) ;
#883 = CARTESIAN_POINT ( 'NONE',  ( -10.00000000000000000, 0.000000000000000000, 0.000000000000000000 ) ) ;
#884 = ORIENTED_EDGE ( 'NONE', *, *, #6432, .T. ) ;
#885 = EDGE_CURVE ( 'NONE', #4827, #274, #3898, .T. ) ;
#886 = DIRECTION ( 'NONE',  ( 0.000000000000000000, 0.000000000000000000, 1.000000000000000000 ) ) ;
#887 = FACE_OUTER_BOUND ( 'NONE', #7832, .T. ) ;
#888 = ORIENTED_EDGE ( 'NONE', *, *, #8564, .F. ) ;
#889 = CARTESIAN_POINT ( 'NONE',  ( -3.411736077305382420, 3.279728542977939476, 8.696051716722022817 ) ) ;
#890 = ORIENTED_EDGE ( 'NONE', *, *, #1809, .T. ) ;
#891 = ORIENTED_EDGE ( 'NONE', *, *, #10393, .F. ) ;
#892 = DIRECTION ( 'NONE',  ( 0.3420201433256627732, -0.9396926207859105373, 0.000000000000000000 ) ) ;
#893 = ORIENTED_EDGE ( 'NONE', *, *, #4207, .F. ) ;
#894 = CARTESIAN_POINT ( 'NONE',  ( -2.625446233515515981, -5.152728359536500768, 4.059999999999999609 ) ) ;
#895 = DIRECTION ( 'NONE',  ( 0.000000000000000000, 0.000000000000000000, -1.000000000000000000 ) ) ;
#896 = CARTESIAN_POINT ( 'NONE',  ( -3.951860609387083834, -3.826313983664940466, 11.60394828327797434 ) ) ;
#897 = VERTEX_POINT ( 'NONE', #10082 ) ;
#898 = CARTESIAN_POINT ( 'NONE',  ( -1.500000000000000222, -13.00000000000000533, -1.312500001365593416 ) ) ;
#899 = ADVANCED_FACE ( 'NONE', ( #10134 ), #10152, .F. ) ;
#900 = ORIENTED_EDGE ( 'NONE', *, *, #447, .F. ) ;
#901 = PLANE ( 'NONE',  #7537 ) ;
#902 = EDGE_CURVE ( 'NONE', #6552, #3003, #8535, .T. ) ;
#903 = DIRECTION ( 'NONE',  ( 1.000000000000000000, 0.000000000000000000, 0.000000000000000000 ) ) ;
#904 = FACE_OUTER_BOUND ( 'NONE', #4621, .T. ) ;
#905 = DIRECTION ( 'NONE',  ( -1.000000000000000000, -0.000000000000000000, 0.000000000000000000 ) ) ;
#906 = VECTOR ( 'NONE', #6253, 1000.000000000000000 ) ;
#907 = CARTESIAN_POINT ( 'NONE',  ( 1.229367062500000163, -12.29022459553277002, -2.802083334016129967 ) ) ;
#908 = CARTESIAN_POINT ( 'NONE',  ( 2.231261971483764484, 4.173491630687871101, 4.463948283277976437 ) ) ;
#909 = VERTEX_POINT ( 'NONE', #6329 ) ;
#910 = CARTESIAN_POINT ( 'NONE',  ( -1.229367062500000163, -12.29022459553277002, -1.135416667349463227 ) ) ;
#911 = CARTESIAN_POINT ( 'NONE',  ( -5.711843387010018702, 0.9046671180729746187, 1.819999999999999396 ) ) ;
#912 = DIRECTION ( 'NONE',  ( 0.000000000000000000, -1.000000000000000000, -0.000000000000000000 ) ) ;
#913 = CIRCLE ( 'NONE', #10073, 6.248999999999999666 ) ;
#914 = CARTESIAN_POINT ( 'NONE',  ( -5.152728359536494551, -2.625446233515535521, 4.339999999999999858 ) ) ;
#915 = CARTESIAN_POINT ( 'NONE',  ( -2.000000000000000000, 8.357095590591340439, 1.552080310331536372 ) ) ;
#916 = DIRECTION ( 'NONE',  ( 0.000000000000000000, 0.000000000000000000, 1.000000000000000000 ) ) ;
#917 = DIRECTION ( 'NONE',  ( 0.000000000000000000, 0.000000000000000000, 1.000000000000000000 ) ) ;
#918 = CARTESIAN_POINT ( 'NONE',  ( 20.71853530928344611, -10.02539999999999942, -12.00000000000000000 ) ) ;
#919 = CARTESIAN_POINT ( 'NONE',  ( 0.8323763977770604061, -4.658724279160015413, 1.976051716722022844 ) ) ;
#920 = FILL_AREA_STYLE_COLOUR ( '', #1541 ) ;
#921 = AXIS2_PLACEMENT_3D ( 'NONE', #4394, #3705, #6721 ) ;
#922 = CARTESIAN_POINT ( 'NONE',  ( -3.244753828200538148, -3.119207202478392116, 3.203948283277977094 ) ) ;
#923 = CARTESIAN_POINT ( 'NONE',  ( 30.00000000000001066, -34.99999999999999289, 9.000000000000000000 ) ) ;
#924 = EDGE_LOOP ( 'NONE', ( #2423, #8115, #5753, #6912 ) ) ;
#925 = EDGE_CURVE ( 'NONE', #10163, #2302, #9097, .T. ) ;
#926 = EDGE_CURVE ( 'NONE', #6166, #7456, #7265, .T. ) ;
#927 =( GEOMETRIC_REPRESENTATION_CONTEXT ( 3 ) GLOBAL_UNCERTAINTY_ASSIGNED_CONTEXT ( ( #6427 ) ) GLOBAL_UNIT_ASSIGNED_CONTEXT ( ( #1683, #96, #6600 ) ) REPRESENTATION_CONTEXT ( 'NONE', 'WORKASPACE' ) );
#928 = VERTEX_POINT ( 'NONE', #1628 ) ;
#929 = DIRECTION ( 'NONE',  ( 1.000000000000000000, 0.000000000000000000, 0.000000000000000000 ) ) ;
#930 = LINE ( 'NONE', #4159, #5259 ) ;
#931 = VERTEX_POINT ( 'NONE', #5011 ) ;
#932 = AXIS2_PLACEMENT_3D ( 'NONE', #1647, #10350, #3 ) ;
#933 = CARTESIAN_POINT ( 'NONE',  ( 4.673326407553653361, -0.7401821875142525764, 3.219999999999999751 ) ) ;
#934 = CARTESIAN_POINT ( 'NONE',  ( 0.000000000000000000, -10.00000000000000000, -12.00000000000000000 ) ) ;
#935 = VERTEX_POINT ( 'NONE', #8255 ) ;
#936 = AXIS2_PLACEMENT_3D ( 'NONE', #6001, #5949, #5215 ) ;
#937 = CARTESIAN_POINT ( 'NONE',  ( -3.411736077305382420, 3.279728542977939476, 5.896051716722023883 ) ) ;
#938 = CARTESIAN_POINT ( 'NONE',  ( 1.499999999999999778, -13.86602540378444637, -1.104166668032260379 ) ) ;
#939 = EDGE_LOOP ( 'NONE', ( #6703, #4676, #5220, #5851 ) ) ;
#940 = EDGE_CURVE ( 'NONE', #2098, #9635, #9900, .T. ) ;
#941 =( NAMED_UNIT ( * ) SI_UNIT ( $, .STERADIAN. ) SOLID_ANGLE_UNIT ( ) );
#942 = VECTOR ( 'NONE', #5802, 1000.000000000000000 ) ;
#943 = ORIENTED_EDGE ( 'NONE', *, *, #1613, .F. ) ;
#944 = DIRECTION ( 'NONE',  ( 0.000000000000000000, 0.000000000000000000, 1.000000000000000000 ) ) ;
#945 = CARTESIAN_POINT ( 'NONE',  ( 5.999999999999999112, -27.00000000000000711, 3.000000000000000000 ) ) ;
#946 = VERTEX_POINT ( 'NONE', #7347 ) ;
#947 = CARTESIAN_POINT ( 'NONE',  ( 0.9046671180729951578, -5.711843387010016926, 3.779999999999998472 ) ) ;
#948 = CARTESIAN_POINT ( 'NONE',  ( 4.900535883036028828, -2.496947748567499126, 6.159999999999999254 ) ) ;
#949 = CARTESIAN_POINT ( 'NONE',  ( -2.496947748567517333, 4.900535883036019058, 2.239999999999999769 ) ) ;
#950 = ORIENTED_EDGE ( 'NONE', *, *, #5479, .T. ) ;
#951 = AXIS2_PLACEMENT_3D ( 'NONE', #8240, #9127, #4244 ) ;
#952 = LINE ( 'NONE', #7413, #2229 ) ;
#953 = VECTOR ( 'NONE', #9625, 1000.000000000000000 ) ;
#954 = ORIENTED_EDGE ( 'NONE', *, *, #7254, .T. ) ;
#955 = CARTESIAN_POINT ( 'NONE',  ( 7.555798540716556211, 6.025400000000000311, -12.00000000000000000 ) ) ;
#956 = LINE ( 'NONE', #800, #10182 ) ;
#957 = CARTESIAN_POINT ( 'NONE',  ( 23.86012795928344588, -10.02539999999999942, -12.00000000000000000 ) ) ;
#958 = ORIENTED_EDGE ( 'NONE', *, *, #5876, .F. ) ;
#959 = DIRECTION ( 'NONE',  ( 0.000000000000000000, 0.000000000000000000, 1.000000000000000000 ) ) ;
#960 = CARTESIAN_POINT ( 'NONE',  ( 0.6146835312499993043, -14.06466310670085562, -1.427083334016129967 ) ) ;
#961 = CARTESIAN_POINT ( 'NONE',  ( 3.244753828200538148, 3.119207202478391672, 4.603948283277976117 ) ) ;
#962 = ORIENTED_EDGE ( 'NONE', *, *, #10068, .T. ) ;
#963 = CARTESIAN_POINT ( 'NONE',  ( 8.000000000000001776, 7.008469740302810891, -0.7425307242147085596 ) ) ;
#964 = CARTESIAN_POINT ( 'NONE',  ( 4.900535883036028828, -2.496947748567499126, 6.159999999999999254 ) ) ;
#965 = CARTESIAN_POINT ( 'NONE',  ( 8.161409553233804459, -10.00000000000000000, -12.00000000000000000 ) ) ;
#966 = CONTEXT_DEPENDENT_SHAPE_REPRESENTATION ( #194, #8188 ) ;
#967 = CARTESIAN_POINT ( 'NONE',  ( -4.089228379062038066, 4.089228379062022078, 4.899999999999999467 ) ) ;
#968 = DIRECTION ( 'NONE',  ( 0.000000000000000000, -0.000000000000000000, 1.000000000000000000 ) ) ;
#969 = CARTESIAN_POINT ( 'NONE',  ( 25.00000000000000000, 0.000000000000000000, -12.00000000000000000 ) ) ;
#970 = CARTESIAN_POINT ( 'NONE',  ( 30.00000000000001066, 35.00000000000001421, 5.999999999999999112 ) ) ;
#971 = CARTESIAN_POINT ( 'NONE',  ( 4.687928535947288644, -0.6479879772514620662, 7.016051716722022213 ) ) ;
#972 = DIRECTION ( 'NONE',  ( 0.000000000000000000, 0.000000000000000000, 1.000000000000000000 ) ) ;
#973 = ADVANCED_FACE ( 'NONE', ( #4956, #8202, #3210 ), #1831, .F. ) ;
#974 = CARTESIAN_POINT ( 'NONE',  ( -3.969226411068985882, 2.122056237541205537, 0.9639482832779766586 ) ) ;
#975 = CARTESIAN_POINT ( 'NONE',  ( 30.00000000000001066, -31.99999999999998579, -6.000000000000000000 ) ) ;
#976 = ORIENTED_EDGE ( 'NONE', *, *, #6674, .T. ) ;
#977 = CARTESIAN_POINT ( 'NONE',  ( 4.155232146225751322, -4.023224611898307934, 1.696051716722023484 ) ) ;
#978 = DIRECTION ( 'NONE',  ( -1.000000000000000000, -0.000000000000000000, -0.000000000000000000 ) ) ;
#979 = CARTESIAN_POINT ( 'NONE',  ( 20.71853530928344611, 6.025400000000000311, -12.00000000000000000 ) ) ;
#980 = VERTEX_POINT ( 'NONE', #1783 ) ;
#981 = CARTESIAN_POINT ( 'NONE',  ( -2.000000000000000000, 0.000000000000000000, 0.000000000000000000 ) ) ;
#982 = PRESENTATION_STYLE_ASSIGNMENT (( #8411 ) ) ;
#983 = ORIENTED_EDGE ( 'NONE', *, *, #3850, .F. ) ;
#984 = EDGE_CURVE ( 'NONE', #5388, #5138, #5355, .T. ) ;
#985 = EDGE_CURVE ( 'NONE', #6306, #614, #8305, .T. ) ;
#986 = CARTESIAN_POINT ( 'NONE',  ( 3.411736077305382420, -3.279728542977940364, 12.89605171672202211 ) ) ;
#987 = CARTESIAN_POINT ( 'NONE',  ( 1.500000000000000222, -13.00000000000000533, -1.062500001365593416 ) ) ;
#988 = ORIENTED_EDGE ( 'NONE', *, *, #5006, .F. ) ;
#989 = ORIENTED_EDGE ( 'NONE', *, *, #6351, .F. ) ;
#990 = CARTESIAN_POINT ( 'NONE',  ( -29.99999999999998934, -13.00000000000000533, 1.249999999999993339 ) ) ;
#991 = ORIENTED_EDGE ( 'NONE', *, *, #529, .F. ) ;
#992 = CARTESIAN_POINT ( 'NONE',  ( -5.418398423912711870, -0.9480714621563917088, 2.676051716722023244 ) ) ;
#993 = CARTESIAN_POINT ( 'NONE',  ( 4.089228379062037178, -4.089228379062022967, 3.499999999999998668 ) ) ;
#994 = CARTESIAN_POINT ( 'NONE',  ( -5.432285873273256627, -0.8603895577212797852, 4.479999999999999538 ) ) ;
#995 = ORIENTED_EDGE ( 'NONE', *, *, #4802, .T. ) ;
#996 = EDGE_CURVE ( 'NONE', #4979, #2729, #8356, .T. ) ;
#997 = CARTESIAN_POINT ( 'NONE',  ( -0.6146835312499998594, -11.93533689329915326, -0.5520833340161299674 ) ) ;
#998 = PRESENTATION_STYLE_ASSIGNMENT (( #4868 ) ) ;
#999 = AXIS2_PLACEMENT_3D ( 'NONE', #8960, #854, #1703 ) ;
#1000 = ORIENTED_EDGE ( 'NONE', *, *, #9190, .T. ) ;
#1001 = DIRECTION ( 'NONE',  ( 0.000000000000000000, 0.000000000000000000, 1.000000000000000000 ) ) ;
#1002 = LINE ( 'NONE', #6167, #3911 ) ;
#1003 = DIRECTION ( 'NONE',  ( 0.3420201433256627732, 0.9396926207859105373, 0.000000000000000000 ) ) ;
#1004 = VERTEX_POINT ( 'NONE', #6263 ) ;
#1005 = CARTESIAN_POINT ( 'NONE',  ( -2.000000000000000000, 6.391777940760639877E-17, 8.843061888689529582 ) ) ;
#1006 = CARTESIAN_POINT ( 'NONE',  ( 1.229367062500000163, -13.00000000000000533, -0.8437500006827965970 ) ) ;
#1007 = CARTESIAN_POINT ( 'NONE',  ( 0.6479879772514793856, -4.687928535947285091, 2.783948283277976277 ) ) ;
#1008 = EDGE_LOOP ( 'NONE', ( #7813, #4123, #3488 ) ) ;
#1009 = CARTESIAN_POINT ( 'NONE',  ( -29.99999999999998934, 0.000000000000000000, 0.000000000000000000 ) ) ;
#1010 = AXIS2_PLACEMENT_3D ( 'NONE', #6074, #2853, #1109 ) ;
#1011 = CARTESIAN_POINT ( 'NONE',  ( 2.496947748567516889, -4.900535883036019946, 0.8399999999999999689 ) ) ;
#1012 = CARTESIAN_POINT ( 'NONE',  ( 0.000000000000000000, 0.000000000000000000, 6.999999999999999112 ) ) ;
#1013 = CARTESIAN_POINT ( 'NONE',  ( -3.889087296526005044, -3.889087296526019255, 9.799999999999998934 ) ) ;
#1014 = CIRCLE ( 'NONE', #9484, 2.500000000000000000 ) ;
#1015 = LINE ( 'NONE', #3457, #6693 ) ;
#1016 = VECTOR ( 'NONE', #8993, 1000.000000000000000 ) ;
#1017 = FACE_OUTER_BOUND ( 'NONE', #1736, .T. ) ;
#1018 = CARTESIAN_POINT ( 'NONE',  ( 8.000000000000001776, 1.459547570502460978, -6.894905428400257996 ) ) ;
#1019 = CARTESIAN_POINT ( 'NONE',  ( -2.122056237541221968, 3.969226411068977889, 6.036051716722022675 ) ) ;
#1020 = CARTESIAN_POINT ( 'NONE',  ( -1.229367062500000163, -12.29022459553277002, -1.510416667349463227 ) ) ;
#1021 = CARTESIAN_POINT ( 'NONE',  ( -2.231261971483764484, -4.173491630687871101, 5.863948283277976792 ) ) ;
#1022 = EDGE_CURVE ( 'NONE', #7942, #6026, #2940, .T. ) ;
#1023 = ADVANCED_FACE ( 'NONE', ( #9629 ), #8663, .T. ) ;
#1024 = CIRCLE ( 'NONE', #9841, 2.000000000000000000 ) ;
#1025 = DIRECTION ( 'NONE',  ( -1.000000000000000000, -0.000000000000000000, -0.000000000000000000 ) ) ;
#1026 = ORIENTED_EDGE ( 'NONE', *, *, #8738, .F. ) ;
#1027 = SHAPE_REPRESENTATION ( 'rack_ISO - Rack-spur - rectangular 1M 20PA 12FW 5PH 25L---SAll', ( #2101 ), #8215 ) ;
#1028 = CARTESIAN_POINT ( 'NONE',  ( 5.726445515403654873, -0.8124729078101852187, 1.416051716722023235 ) ) ;
#1029 = MANIFOLD_SOLID_BREP ( 'Move Face1', #843 ) ;
#1030 = AXIS2_PLACEMENT_3D ( 'NONE', #8223, #1546, #7416 ) ;
#1031 = CYLINDRICAL_SURFACE ( 'NONE', #2899, 8.500000000000000000 ) ;
#1032 = VECTOR ( 'NONE', #3301, 1000.000000000000000 ) ;
#1033 = EDGE_CURVE ( 'NONE', #1639, #6225, #3260, .T. ) ;
#1034 = DIRECTION ( 'NONE',  ( -0.9396926207859105373, -0.3420201433256627732, 0.000000000000000000 ) ) ;
#1035 = ORIENTED_EDGE ( 'NONE', *, *, #7193, .T. ) ;
#1036 = CARTESIAN_POINT ( 'NONE',  ( 5.838749930332745919, 3.750000000000000000, -12.00000000000000000 ) ) ;
#1037 = VECTOR ( 'NONE', #7003, 1000.000000000000000 ) ;
#1038 = FILL_AREA_STYLE ('',( #3422 ) ) ;
#1039 = EDGE_LOOP ( 'NONE', ( #4958, #5026 ) ) ;
#1040 = CARTESIAN_POINT ( 'NONE',  ( 4.430710083317573655, 0.7916369971161595354, 9.676051716722021467 ) ) ;
#1041 = AXIS2_PLACEMENT_3D ( 'NONE', #6956, #8405, #294 ) ;
#1042 = CARTESIAN_POINT ( 'NONE',  ( 1.229367062500000163, -13.00000000000000533, -2.343750000682796486 ) ) ;
#1043 = ORIENTED_EDGE ( 'NONE', *, *, #4936, .F. ) ;
#1044 = FILL_AREA_STYLE ('',( #6051 ) ) ;
#1045 = ORIENTED_EDGE ( 'NONE', *, *, #3799, .F. ) ;
#1046 = DIRECTION ( 'NONE',  ( -0.000000000000000000, -0.000000000000000000, -1.000000000000000000 ) ) ;
#1047 = EDGE_CURVE ( 'NONE', #8424, #3846, #3537, .T. ) ;
#1048 = DIRECTION ( 'NONE',  ( 0.000000000000000000, 0.000000000000000000, 1.000000000000000000 ) ) ;
#1049 = ORIENTED_EDGE ( 'NONE', *, *, #4497, .T. ) ;
#1050 = CARTESIAN_POINT ( 'NONE',  ( -0.9968613283357868893, 5.697241258616382531, 3.376051716722022977 ) ) ;
#1051 = CARTESIAN_POINT ( 'NONE',  ( 2.625446233515515537, 5.152728359536502545, 8.259999999999999787 ) ) ;
#1052 = CARTESIAN_POINT ( 'NONE',  ( -3.889087296526005044, -3.889087296526019255, 12.59999999999999787 ) ) ;
#1053 = ORIENTED_EDGE ( 'NONE', *, *, #3828, .T. ) ;
#1054 = CARTESIAN_POINT ( 'NONE',  ( -1.229367062500000163, -13.00000000000000533, -1.468750000682796486 ) ) ;
#1055 = PRESENTATION_STYLE_ASSIGNMENT (( #6067 ) ) ;
#1056 = EDGE_LOOP ( 'NONE', ( #5495, #10274, #1904, #8832 ) ) ;
#1057 = EDGE_CURVE ( 'NONE', #7824, #1146, #602, .T. ) ;
#1058 = DIRECTION ( 'NONE',  ( 0.000000000000000000, 0.000000000000000000, 1.000000000000000000 ) ) ;
#1059 = EDGE_CURVE ( 'NONE', #4252, #2255, #10372, .T. ) ;
#1060 = LINE ( 'NONE', #9872, #9831 ) ;
#1061 = VERTEX_POINT ( 'NONE', #6314 ) ;
#1062 = PLANE ( 'NONE',  #4221 ) ;
#1063 = CARTESIAN_POINT ( 'NONE',  ( -1.229367062500000163, -12.29022459553277002, -0.6354166673494632267 ) ) ;
#1064 = CARTESIAN_POINT ( 'NONE',  ( -4.258245684917310925, -2.064922774268914019, 11.74394828327797846 ) ) ;
#1065 = ORIENTED_EDGE ( 'NONE', *, *, #5251, .F. ) ;
#1066 = DIRECTION ( 'NONE',  ( 0.3420201433256627732, -0.9396926207859105373, 0.000000000000000000 ) ) ;
#1067 = PLANE ( 'NONE',  #1259 ) ;
#1068 = CARTESIAN_POINT ( 'NONE',  ( 6.727620669667255804, 3.750000000000000000, -12.00000000000000000 ) ) ;
#1069 = EDGE_CURVE ( 'NONE', #3641, #9420, #7060, .T. ) ;
#1070 = CARTESIAN_POINT ( 'NONE',  ( -4.900535883036028828, 2.496947748567499126, 7.559999999999998721 ) ) ;
#1071 = VECTOR ( 'NONE', #1221, 1000.000000000000000 ) ;
#1072 = CARTESIAN_POINT ( 'NONE',  ( 0.000000000000000000, 0.000000000000000000, 3.000000000000000000 ) ) ;
#1073 = CYLINDRICAL_SURFACE ( 'NONE', #2483, 1.500000000000000222 ) ;
#1074 = CARTESIAN_POINT ( 'NONE',  ( 1.500000000000000222, -13.00000000000000533, -3.000000000000000000 ) ) ;
#1075 = CARTESIAN_POINT ( 'NONE',  ( -0.9968613283357868893, 5.697241258616382531, 14.57605171672202538 ) ) ;
#1076 = CARTESIAN_POINT ( 'NONE',  ( 0.6146835312500001924, -11.93533689329915326, -2.135416667349463449 ) ) ;
#1077 = CARTESIAN_POINT ( 'NONE',  ( -4.023224611898323033, 4.155232146225737111, 1.103948283277976561 ) ) ;
#1078 = CIRCLE ( 'NONE', #3283, 1.280000000000000027 ) ;
#1079 = CARTESIAN_POINT ( 'NONE',  ( 1.229367062500000163, -13.00000000000000533, -2.218750000682796486 ) ) ;
#1080 = ORIENTED_EDGE ( 'NONE', *, *, #2708, .F. ) ;
#1081 = CARTESIAN_POINT ( 'NONE',  ( 5.726445515403654873, -0.8124729078101852187, 4.216051716722023279 ) ) ;
#1082 = DIRECTION ( 'NONE',  ( 0.000000000000000000, 0.000000000000000000, 1.000000000000000000 ) ) ;
#1083 = FACE_OUTER_BOUND ( 'NONE', #3328, .T. ) ;
#1084 = ORIENTED_EDGE ( 'NONE', *, *, #6222, .F. ) ;
#1085 = AXIS2_PLACEMENT_3D ( 'NONE', #9340, #1919, #1275 ) ;
#1086 = CARTESIAN_POINT ( 'NONE',  ( -4.444597532678119300, -0.7039550926810477227, 7.279999999999999361 ) ) ;
#1087 = CARTESIAN_POINT ( 'NONE',  ( 3.411736077305382420, -3.279728542977940364, 4.496051716722022640 ) ) ;
#1088 =( BOUNDED_CURVE ( )  B_SPLINE_CURVE ( 2, ( #8758, #1499, #6470, #3992, #9727, #9676, #2406, #18, #4720, #706, #5623, #7162, #10419, #2346, #5569, #1559, #8817, #1609, #810, #4040, #7271, #2458, #5673, #10042, #9126, #1816, #4141, #172, #5877, #9183, #6631, #914, #7489, #1867, #7427, #967, #4193, #8342, #229, #1920, #6783, #3406, #1714, #9883, #3556, #5092, #2763, #7583, #2561, #9081, #2613, #1122, #5144, #5828, #1070, #4344, #327, #5929, #5978, #1763, #4940, #5040, #3505, #9830, #8182, #8238, #8287, #123, #4243, #281, #1013, #7536, #6722, #6574, #8391, #4293, #3456, #6677, #7379, #9026, #3348, #5776, #9935, #2661, #9985, #2710, #4990, #2075, #10194, #2021, #2973, #7644, #2921, #3022, #9447, #2176, #10293, #9235, #1167, #4395, #4550 ),
 .UNSPECIFIED., .F., .T. ) 
 B_SPLINE_CURVE_WITH_KNOTS ( ( 3, 2, 2, 2, 2, 2, 2, 2, 2, 2, 2, 2, 2, 2, 2, 2, 2, 2, 2, 2, 2, 2, 2, 2, 2, 2, 2, 2, 2, 2, 2, 2, 2, 2, 2, 2, 2, 2, 2, 2, 2, 2, 2, 2, 2, 2, 2, 2, 2, 2, 3 ),
 ( 0.000000000000000000, 0.02000000000000000042, 0.04000000000000000083, 0.05999999999999999778, 0.08000000000000000167, 0.1000000000000000056, 0.1199999999999999956, 0.1400000000000000133, 0.1600000000000000033, 0.1799999999999999933, 0.2000000000000000111, 0.2200000000000000011, 0.2399999999999999911, 0.2600000000000000089, 0.2800000000000000266, 0.2999999999999999889, 0.3200000000000000067, 0.3400000000000000244, 0.3599999999999999867, 0.3800000000000000044, 0.4000000000000000222, 0.4199999999999999845, 0.4400000000000000022, 0.4600000000000000200, 0.4799999999999999822, 0.5000000000000000000, 0.5200000000000000178, 0.5400000000000000355, 0.5600000000000000533, 0.5799999999999999600, 0.5999999999999999778, 0.6199999999999999956, 0.6400000000000000133, 0.6600000000000000311, 0.6800000000000000488, 0.6999999999999999556, 0.7199999999999999734, 0.7399999999999999911, 0.7600000000000000089, 0.7800000000000000266, 0.8000000000000000444, 0.8199999999999999512, 0.8399999999999999689, 0.8599999999999999867, 0.8800000000000000044, 0.9000000000000000222, 0.9200000000000000400, 0.9399999999999999467, 0.9599999999999999645, 0.9799999999999999822, 1.000000000000000000 ),
 .UNSPECIFIED. ) 
 CURVE ( )  GEOMETRIC_REPRESENTATION_ITEM ( )  RATIONAL_B_SPLINE_CURVE ( ( 1.000000000000000000, 0.9510565162951535312, 1.000000000000000000, 0.9510565162951535312, 1.000000000000000000, 0.9510565162951535312, 1.000000000000000000, 0.9510565162951535312, 1.000000000000000000, 0.9510565162951535312, 1.000000000000000000, 0.9510565162951535312, 1.000000000000000000, 0.9510565162951535312, 1.000000000000000000, 0.9510565162951535312, 1.000000000000000000, 0.9510565162951535312, 1.000000000000000000, 0.9510565162951535312, 1.000000000000000000, 0.9510565162951535312, 1.000000000000000000, 0.9510565162951535312, 1.000000000000000000, 0.9510565162951535312, 1.000000000000000000, 0.9510565162951535312, 1.000000000000000000, 0.9510565162951535312, 1.000000000000000000, 0.9510565162951535312, 1.000000000000000000, 0.9510565162951535312, 1.000000000000000000, 0.9510565162951535312, 1.000000000000000000, 0.9510565162951535312, 1.000000000000000000, 0.9510565162951535312, 1.000000000000000000, 0.9510565162951535312, 1.000000000000000000, 0.9510565162951535312, 1.000000000000000000, 0.9510565162951535312, 1.000000000000000000, 0.9510565162951535312, 1.000000000000000000, 0.9510565162951535312, 1.000000000000000000, 0.9510565162951535312, 1.000000000000000000, 0.9510565162951535312, 1.000000000000000000, 0.9510565162951535312, 1.000000000000000000, 0.9510565162951535312, 1.000000000000000000, 0.9510565162951535312, 1.000000000000000000, 0.9510565162951535312, 1.000000000000000000, 0.9510565162951535312, 1.000000000000000000, 0.9510565162951535312, 1.000000000000000000, 0.9510565162951535312, 1.000000000000000000, 0.9510565162951535312, 1.000000000000000000, 0.9510565162951535312, 1.000000000000000000, 0.9510565162951535312, 1.000000000000000000, 0.9510565162951535312, 1.000000000000000000, 0.9510565162951535312, 1.000000000000000000, 0.9510565162951535312, 1.000000000000000000, 0.9510565162951535312, 1.000000000000000000, 0.9510565162951535312, 1.000000000000000000, 0.9510565162951535312, 1.000000000000000000, 0.9510565162951535312, 1.000000000000000000, 0.9510565162951535312, 1.000000000000000000, 0.9510565162951535312, 1.000000000000000000, 0.9510565162951535312, 1.000000000000000000, 0.9510565162951535312, 1.000000000000000000, 0.9510565162951535312, 1.000000000000000000, 0.9510565162951535312, 1.000000000000000000 ) ) 
 REPRESENTATION_ITEM ( '' )  );
#1089 = CARTESIAN_POINT ( 'NONE',  ( 1.229367062500000385, -12.29022459553277002, -2.802083334016129523 ) ) ;
#1090 = ORIENTED_EDGE ( 'NONE', *, *, #595, .T. ) ;
#1091 =( NAMED_UNIT ( * ) PLANE_ANGLE_UNIT ( ) SI_UNIT ( $, .RADIAN. ) );
#1092 = ORIENTED_EDGE ( 'NONE', *, *, #2254, .T. ) ;
#1093 = DIRECTION ( 'NONE',  ( 0.3420201433256627732, 0.9396926207859105373, 0.000000000000000000 ) ) ;
#1094 = VECTOR ( 'NONE', #2863, 1000.000000000000000 ) ;
#1095 = CARTESIAN_POINT ( 'NONE',  ( -1.500000000000000222, -13.00000000000000533, -0.2500000000000002220 ) ) ;
#1096 = VERTEX_POINT ( 'NONE', #4727 ) ;
#1097 = CARTESIAN_POINT ( 'NONE',  ( 5.152728359536493663, 2.625446233515533745, 11.33999999999999808 ) ) ;
#1098 = CARTESIAN_POINT ( 'NONE',  ( -5.432285873273256627, -0.8603895577212797852, 1.679999999999999938 ) ) ;
#1099 = CARTESIAN_POINT ( 'NONE',  ( 0.9046671180729951578, -5.711843387010016926, 9.379999999999995453 ) ) ;
#1100 = EDGE_LOOP ( 'NONE', ( #4005, #10378, #7221, #10183 ) ) ;
#1101 = CARTESIAN_POINT ( 'NONE',  ( 8.692241771943169307E-17, -11.58044919106553294, -1.593750000682796486 ) ) ;
#1102 = VECTOR ( 'NONE', #3758, 1000.000000000000000 ) ;
#1103 = ADVANCED_FACE ( 'NONE', ( #7979 ), #5367, .T. ) ;
#1104 =( GEOMETRIC_REPRESENTATION_CONTEXT ( 3 ) GLOBAL_UNCERTAINTY_ASSIGNED_CONTEXT ( ( #2307 ) ) GLOBAL_UNIT_ASSIGNED_CONTEXT ( ( #2584, #9704, #941 ) ) REPRESENTATION_CONTEXT ( 'NONE', 'WORKASPACE' ) );
#1105 = ORIENTED_EDGE ( 'NONE', *, *, #3056, .F. ) ;
#1106 = CARTESIAN_POINT ( 'NONE',  ( -1.500000000000000222, -13.00000000000000533, -2.750000000000000000 ) ) ;
#1107 = CARTESIAN_POINT ( 'NONE',  ( -1.499999999999996669, -12.13397459621556607, -0.8541666680322607119 ) ) ;
#1108 = ORIENTED_EDGE ( 'NONE', *, *, #9516, .F. ) ;
#1109 = DIRECTION ( 'NONE',  ( 0.000000000000000000, 0.000000000000000000, 1.000000000000000000 ) ) ;
#1110 = AXIS2_PLACEMENT_3D ( 'NONE', #9054, #3327, #4117 ) ;
#1111 = CARTESIAN_POINT ( 'NONE',  ( 1.300000000000000044, -0.7390083445627225744, -1.279999999999999138 ) ) ;
#1112 = CARTESIAN_POINT ( 'NONE',  ( -1.229367062500000163, -13.00000000000000533, -2.093750000682796930 ) ) ;
#1113 = CARTESIAN_POINT ( 'NONE',  ( 0.6479879772514793856, -4.687928535947285091, 11.18394828327797441 ) ) ;
#1114 = EDGE_LOOP ( 'NONE', ( #5375, #5317, #9863, #4627 ) ) ;
#1115 = CIRCLE ( 'NONE', #6179, 6.248999999999999666 ) ;
#1116 = DIRECTION ( 'NONE',  ( 0.3420201433256627732, 0.9396926207859105373, -0.000000000000000000 ) ) ;
#1117 = ADVANCED_FACE ( 'NONE', ( #3941 ), #1519, .F. ) ;
#1118 = EDGE_CURVE ( 'NONE', #8741, #1470, #4721, .T. ) ;
#1119 = CARTESIAN_POINT ( 'NONE',  ( -4.900535883036028828, 2.496947748567499126, 10.35999999999999943 ) ) ;
#1120 = PLANE ( 'NONE',  #1762 ) ;
#1121 = AXIS2_PLACEMENT_3D ( 'NONE', #9084, #5777, #4345 ) ;
#1122 = CARTESIAN_POINT ( 'NONE',  ( -5.152728359536494551, -2.625446233515535521, 7.139999999999998792 ) ) ;
#1123 = VECTOR ( 'NONE', #2714, 1000.000000000000000 ) ;
#1124 = PLANE ( 'NONE',  #9242 ) ;
#1125 = DIRECTION ( 'NONE',  ( 0.000000000000000000, 0.000000000000000000, 1.000000000000000000 ) ) ;
#1126 = DIRECTION ( 'NONE',  ( -0.000000000000000000, -0.000000000000000000, -1.000000000000000000 ) ) ;
#1127 = CARTESIAN_POINT ( 'NONE',  ( -4.444597532678119300, -0.7039550926810477227, 1.679999999999999938 ) ) ;
#1128 = CARTESIAN_POINT ( 'NONE',  ( 0.6146835312500001924, -11.93533689329915326, -1.135416667349463227 ) ) ;
#1129 = ADVANCED_FACE ( 'NONE', ( #1340 ), #2146, .T. ) ;
#1130 = CARTESIAN_POINT ( 'NONE',  ( 0.9480714621563713917, 5.418398423912717199, 1.523948283277976268 ) ) ;
#1131 = CARTESIAN_POINT ( 'NONE',  ( 0.6146835312499993043, -14.06466310670085562, -1.802083334016129745 ) ) ;
#1132 = ORIENTED_EDGE ( 'NONE', *, *, #3008, .T. ) ;
#1133 = CARTESIAN_POINT ( 'NONE',  ( -5.726445515403654873, 0.8124729078101847746, 8.416051716722021681 ) ) ;
#1134 = DIRECTION ( 'NONE',  ( -1.000000000000000000, 0.000000000000000000, -0.000000000000000000 ) ) ;
#1135 = LINE ( 'NONE', #8453, #8483 ) ;
#1136 = EDGE_LOOP ( 'NONE', ( #3793, #943, #1240, #4213 ) ) ;
#1137 = CARTESIAN_POINT ( 'NONE',  ( -3.181980515339458027, -3.181980515339470905, 6.999999999999999112 ) ) ;
#1138 = FACE_OUTER_BOUND ( 'NONE', #7007, .T. ) ;
#1139 = CARTESIAN_POINT ( 'NONE',  ( 3.345732310141667387, -3.345732310141653620, 0.6999999999999997335 ) ) ;
#1140 = CARTESIAN_POINT ( 'NONE',  ( 7.546553696766195252, 6.000000000000000000, 0.000000000000000000 ) ) ;
#1141 = ORIENTED_EDGE ( 'NONE', *, *, #1425, .T. ) ;
#1142 = DIRECTION ( 'NONE',  ( 0.000000000000000000, 0.000000000000000000, 1.000000000000000000 ) ) ;
#1143 = ORIENTED_EDGE ( 'NONE', *, *, #9914, .T. ) ;
#1144 = CARTESIAN_POINT ( 'NONE',  ( 25.00000000000000000, 0.000000000000000000, 0.000000000000000000 ) ) ;
#1145 = DIRECTION ( 'NONE',  ( 1.000000000000000000, 0.000000000000000000, 0.000000000000000000 ) ) ;
#1146 = VERTEX_POINT ( 'NONE', #3354 ) ;
#1147 = CARTESIAN_POINT ( 'NONE',  ( 0.8603895577212593571, 5.432285873273261068, 13.71999999999999886 ) ) ;
#1148 = CARTESIAN_POINT ( 'NONE',  ( -3.889087296526005044, -3.889087296526019255, 9.799999999999998934 ) ) ;
#1149 = CARTESIAN_POINT ( 'NONE',  ( -4.900535883036028828, 2.496947748567499126, 13.15999999999999837 ) ) ;
#1150 = ORIENTED_EDGE ( 'NONE', *, *, #5004, .T. ) ;
#1151 = CARTESIAN_POINT ( 'NONE',  ( -2.607672531582950546E-16, -14.41955080893447416, 0.1562499993172034585 ) ) ;
#1152 = EDGE_CURVE ( 'NONE', #4358, #7070, #4378, .T. ) ;
#1153 = ORIENTED_EDGE ( 'NONE', *, *, #4265, .F. ) ;
#1154 = LINE ( 'NONE', #10030, #1441 ) ;
#1155 = DIRECTION ( 'NONE',  ( 1.000000000000000000, 0.000000000000000000, 0.000000000000000000 ) ) ;
#1156 = ORIENTED_EDGE ( 'NONE', *, *, #6616, .T. ) ;
#1157 = DIRECTION ( 'NONE',  ( -0.000000000000000000, -0.000000000000000000, 1.000000000000000000 ) ) ;
#1158 = EDGE_CURVE ( 'NONE', #6291, #5295, #5727, .T. ) ;
#1159 = DIRECTION ( 'NONE',  ( 0.000000000000000000, 1.000000000000000000, 0.000000000000000000 ) ) ;
#1160 = CARTESIAN_POINT ( 'NONE',  ( -1.229367062500000163, -13.00000000000000533, -1.593750000682796708 ) ) ;
#1161 = CARTESIAN_POINT ( 'NONE',  ( -0.7916369971161423269, -4.430710083317576320, 5.723948283277976223 ) ) ;
#1162 = ORIENTED_EDGE ( 'NONE', *, *, #787, .F. ) ;
#1163 = DIRECTION ( 'NONE',  ( 0.3420201433256627732, 0.9396926207859105373, -0.000000000000000000 ) ) ;
#1164 = VECTOR ( 'NONE', #3927, 1000.000000000000000 ) ;
#1165 = CARTESIAN_POINT ( 'NONE',  ( 4.089228379062037178, -4.089228379062022967, 11.90000000000000036 ) ) ;
#1166 = FACE_BOUND ( 'NONE', #3116, .T. ) ;
#1167 = CARTESIAN_POINT ( 'NONE',  ( 0.8603895577212593571, 5.432285873273261068, 13.71999999999999886 ) ) ;
#1168 = DIRECTION ( 'NONE',  ( 0.3420201433256627732, -0.9396926207859105373, 0.000000000000000000 ) ) ;
#1169 = EDGE_CURVE ( 'NONE', #5388, #2194, #3876, .T. ) ;
#1170 = DIRECTION ( 'NONE',  ( -1.000000000000000000, 0.000000000000000000, -0.000000000000000000 ) ) ;
#1171 = EDGE_CURVE ( 'NONE', #1096, #1785, #5782, .T. ) ;
#1172 = COLOUR_RGB ( '', 0.09019608, 0.27058824, 0.51372549) ;
#1173 = LINE ( 'NONE', #9286, #171 ) ;
#1174 = CARTESIAN_POINT ( 'NONE',  ( -4.173491630687863108, -2.231261971483782691, 10.93605171672202125 ) ) ;
#1175 = VECTOR ( 'NONE', #4384, 1000.000000000000000 ) ;
#1176 = CARTESIAN_POINT ( 'NONE',  ( -0.6146835312500006365, -14.06466310670085562, -0.8854166673494632267 ) ) ;
#1177 = CARTESIAN_POINT ( 'NONE',  ( -3.951860609387083834, -3.826313983664940466, 3.203948283277977094 ) ) ;
#1178 = CARTESIAN_POINT ( 'NONE',  ( -1.229367062500000163, -13.00000000000000533, -0.4687500006827967081 ) ) ;
#1179 = CIRCLE ( 'NONE', #7790, 0.5000000000000000000 ) ;
#1180 = ORIENTED_EDGE ( 'NONE', *, *, #6685, .T. ) ;
#1181 = COLOUR_RGB ( '', 0.09019608, 0.27058824, 0.51372549) ;
#1182 = CARTESIAN_POINT ( 'NONE',  ( -2.576046737280769605, 4.860232935257343456, 6.036051716722022675 ) ) ;
#1183 = EDGE_CURVE ( 'NONE', #1730, #9404, #8033, .T. ) ;
#1184 = CARTESIAN_POINT ( 'NONE',  ( 10.00000000000000000, -7.009698679648292519, 0.7308381473896652381 ) ) ;
#1185 = DIRECTION ( 'NONE',  ( 0.000000000000000000, 0.000000000000000000, -1.000000000000000000 ) ) ;
#1186 = ORIENTED_EDGE ( 'NONE', *, *, #1304, .T. ) ;
#1187 =( GEOMETRIC_REPRESENTATION_CONTEXT ( 3 ) GLOBAL_UNCERTAINTY_ASSIGNED_CONTEXT ( ( #1667 ) ) GLOBAL_UNIT_ASSIGNED_CONTEXT ( ( #10273, #1625, #3157 ) ) REPRESENTATION_CONTEXT ( 'NONE', 'WORKASPACE' ) );
#1188 = CARTESIAN_POINT ( 'NONE',  ( 0.7039550926810297371, 4.444597532678122853, 10.91999999999999993 ) ) ;
#1189 = CARTESIAN_POINT ( 'NONE',  ( -29.99999999999998934, -35.00000000000000000, -9.000000000000000000 ) ) ;
#1190 = VECTOR ( 'NONE', #3780, 1000.000000000000000 ) ;
#1191 = CARTESIAN_POINT ( 'NONE',  ( -0.8323763977770610722, 4.658724279160015413, 14.57605171672202538 ) ) ;
#1192 = CARTESIAN_POINT ( 'NONE',  ( 0.6146835312499993043, -14.06466310670085562, 0.07291666598386974119 ) ) ;
#1193 = ORIENTED_EDGE ( 'NONE', *, *, #529, .T. ) ;
#1194 = CARTESIAN_POINT ( 'NONE',  ( 0.000000000000000000, 0.000000000000000000, -30.00000000000000000 ) ) ;
#1195 = VECTOR ( 'NONE', #7864, 1000.000000000000000 ) ;
#1196 = ORIENTED_EDGE ( 'NONE', *, *, #1425, .F. ) ;
#1197 = EDGE_CURVE ( 'NONE', #8501, #9821, #4045, .T. ) ;
#1198 = LINE ( 'NONE', #6752, #3147 ) ;
#1199 = DIRECTION ( 'NONE',  ( -1.000000000000000000, -0.000000000000000000, -0.000000000000000000 ) ) ;
#1200 = AXIS2_PLACEMENT_3D ( 'NONE', #6027, #9278, #2017 ) ;
#1201 = DIRECTION ( 'NONE',  ( 1.000000000000000000, 0.000000000000000000, 0.000000000000000000 ) ) ;
#1202 = ORIENTED_EDGE ( 'NONE', *, *, #1450, .T. ) ;
#1203 = CARTESIAN_POINT ( 'NONE',  ( -5.152728359536494551, -2.625446233515535077, 12.73999999999999488 ) ) ;
#1204 = CARTESIAN_POINT ( 'NONE',  ( 5.711843387010018702, -0.9046671180729751738, 11.61999999999999922 ) ) ;
#1205 = AXIS2_PLACEMENT_3D ( 'NONE', #8466, #2153, #4579 ) ;
#1206 = CARTESIAN_POINT ( 'NONE',  ( 2.625446233515515537, 5.152728359536502545, 8.259999999999999787 ) ) ;
#1207 = ORIENTED_EDGE ( 'NONE', *, *, #4683, .F. ) ;
#1208 = DIRECTION ( 'NONE',  ( -0.000000000000000000, 0.000000000000000000, 1.000000000000000000 ) ) ;
#1209 = UNCERTAINTY_MEASURE_WITH_UNIT (LENGTH_MEASURE( 1.000000000000000082E-05 ), #6662, 'distance_accuracy_value', 'NONE');
#1210 = SURFACE_STYLE_FILL_AREA ( #5126 ) ;
#1211 = VERTEX_POINT ( 'NONE', #875 ) ;
#1212 = CARTESIAN_POINT ( 'NONE',  ( 14.43535000928344481, 6.025400000000000311, -12.00000000000000000 ) ) ;
#1213 = FACE_OUTER_BOUND ( 'NONE', #9376, .T. ) ;
#1214 = ORIENTED_EDGE ( 'NONE', *, *, #9476, .T. ) ;
#1215 = CYLINDRICAL_SURFACE ( 'NONE', #5234, 2.000000000000000000 ) ;
#1216 = PLANE ( 'NONE',  #6136 ) ;
#1217 = CARTESIAN_POINT ( 'NONE',  ( 8.000000000000001776, 0.000000000000000000, 0.000000000000000000 ) ) ;
#1218 = CARTESIAN_POINT ( 'NONE',  ( -2.231261971483764484, -4.173491630687871101, 8.663948283277974838 ) ) ;
#1219 = ORIENTED_EDGE ( 'NONE', *, *, #150, .T. ) ;
#1220 = LINE ( 'NONE', #4499, #6090 ) ;
#1221 = DIRECTION ( 'NONE',  ( 0.3420201433256627732, -0.9396926207859105373, 0.000000000000000000 ) ) ;
#1222 = FACE_BOUND ( 'NONE', #1039, .T. ) ;
#1223 = EDGE_CURVE ( 'NONE', #9435, #3589, #5730, .T. ) ;
#1224 = CARTESIAN_POINT ( 'NONE',  ( -2.000000000000000000, 8.265874651078044977, -1.981241088980697729 ) ) ;
#1225 = CYLINDRICAL_SURFACE ( 'NONE', #2645, 2.000000000000000000 ) ;
#1226 = FACE_OUTER_BOUND ( 'NONE', #924, .T. ) ;
#1227 = DIRECTION ( 'NONE',  ( -1.000000000000000000, -0.000000000000000000, -0.000000000000000000 ) ) ;
#1228 = CARTESIAN_POINT ( 'NONE',  ( 2.064922774268895811, 4.258245684917319807, 14.85605171672202296 ) ) ;
#1229 = CARTESIAN_POINT ( 'NONE',  ( -0.6146835312499998594, -11.93533689329915326, -2.052083334016129967 ) ) ;
#1230 = CARTESIAN_POINT ( 'NONE',  ( 0.7916369971161419938, 4.430710083317576320, 9.923948283277976401 ) ) ;
#1231 = CARTESIAN_POINT ( 'NONE',  ( -0.6146835312499998594, -11.93533689329915326, -2.052083334016129967 ) ) ;
#1232 = ADVANCED_FACE ( 'NONE', ( #4199 ), #9733, .F. ) ;
#1233 = ORIENTED_EDGE ( 'NONE', *, *, #6350, .F. ) ;
#1234 = CIRCLE ( 'NONE', #1746, 3.000000000000000000 ) ;
#1235 = DIRECTION ( 'NONE',  ( 1.000000000000000000, 0.000000000000000000, 0.000000000000000000 ) ) ;
#1236 = MANIFOLD_SOLID_BREP ( 'Hex', #1694 ) ;
#1237 = CARTESIAN_POINT ( 'NONE',  ( -10.00000000000000000, 0.000000000000000000, 0.000000000000000000 ) ) ;
#1238 = CARTESIAN_POINT ( 'NONE',  ( 20.11292429676619520, 6.000000000000000000, 0.000000000000000000 ) ) ;
#1239 = DIRECTION ( 'NONE',  ( 0.000000000000000000, 0.000000000000000000, 1.000000000000000000 ) ) ;
#1240 = ORIENTED_EDGE ( 'NONE', *, *, #2513, .F. ) ;
#1241 = CARTESIAN_POINT ( 'NONE',  ( -4.444597532678119300, -0.7039550926810477227, 12.87999999999999901 ) ) ;
#1242 = CIRCLE ( 'NONE', #1595, 2.000000000000001776 ) ;
#1243 = DIRECTION ( 'NONE',  ( -0.000000000000000000, -0.000000000000000000, 1.000000000000000000 ) ) ;
#1244 = CARTESIAN_POINT ( 'NONE',  ( 3.345732310141667387, -3.345732310141653620, 6.299999999999999822 ) ) ;
#1245 = ADVANCED_FACE ( 'NONE', ( #3200 ), #8245, .F. ) ;
#1246 = CARTESIAN_POINT ( 'NONE',  ( -0.6146835312499998594, -11.93533689329915326, -0.1770833340161300506 ) ) ;
#1247 = EDGE_CURVE ( 'NONE', #1286, #8006, #1362, .T. ) ;
#1248 = VERTEX_POINT ( 'NONE', #9686 ) ;
#1249 = ORIENTED_EDGE ( 'NONE', *, *, #4265, .T. ) ;
#1250 = DIRECTION ( 'NONE',  ( -0.000000000000000000, -1.000000000000000000, -0.000000000000000000 ) ) ;
#1251 = DIRECTION ( 'NONE',  ( -1.000000000000000000, -1.156482317317871478E-16, 5.204170427930421283E-15 ) ) ;
#1252 = DIRECTION ( 'NONE',  ( 0.000000000000000000, -0.000000000000000000, 1.000000000000000000 ) ) ;
#1253 = ORIENTED_EDGE ( 'NONE', *, *, #7964, .T. ) ;
#1254 = CARTESIAN_POINT ( 'NONE',  ( -4.155232146225753098, 4.023224611898306158, 8.696051716722022817 ) ) ;
#1255 = CARTESIAN_POINT ( 'NONE',  ( -4.089228379062038066, 4.089228379062021190, 10.50000000000000000 ) ) ;
#1256 = CARTESIAN_POINT ( 'NONE',  ( -4.089228379062038066, 4.089228379062021190, 4.900000000000000355 ) ) ;
#1257 = ORIENTED_EDGE ( 'NONE', *, *, #398, .T. ) ;
#1258 = DIRECTION ( 'NONE',  ( 0.000000000000000000, 0.000000000000000000, 1.000000000000000000 ) ) ;
#1259 = AXIS2_PLACEMENT_3D ( 'NONE', #3503, #5874, #1970 ) ;
#1260 = EDGE_CURVE ( 'NONE', #798, #4172, #4077, .T. ) ;
#1261 = ORIENTED_EDGE ( 'NONE', *, *, #9693, .T. ) ;
#1262 = CARTESIAN_POINT ( 'NONE',  ( 27.00000000000001066, -25.00000000000000000, 1.999999999999997780 ) ) ;
#1263 = COLOUR_RGB ( '', 0.08235294, 0.09019608, 0.10196078) ;
#1264 = DIRECTION ( 'NONE',  ( 1.000000000000000000, 0.000000000000000000, 0.000000000000000000 ) ) ;
#1265 = ORIENTED_EDGE ( 'NONE', *, *, #6212, .T. ) ;
#1266 = CARTESIAN_POINT ( 'NONE',  ( 10.68814634676619590, 6.000000000000000000, -12.00000000000000000 ) ) ;
#1267 = CARTESIAN_POINT ( 'NONE',  ( 5.999999999999999112, 26.99999999999999289, -14.00000000000000178 ) ) ;
#1268 = CARTESIAN_POINT ( 'NONE',  ( -0.7916369971161423269, -4.430710083317576320, 8.523948283277976046 ) ) ;
#1269 = ORIENTED_EDGE ( 'NONE', *, *, #2149, .F. ) ;
#1270 = VECTOR ( 'NONE', #8747, 1000.000000000000000 ) ;
#1271 = CARTESIAN_POINT ( 'NONE',  ( 10.00000000000000000, 0.000000000000000000, 0.000000000000000000 ) ) ;
#1272 =( REPRESENTATION_RELATIONSHIP ('NONE','NONE', #5100, #7207 ) REPRESENTATION_RELATIONSHIP_WITH_TRANSFORMATION ( #8970 )SHAPE_REPRESENTATION_RELATIONSHIP( ) );
#1273 = LINE ( 'NONE', #8489, #1071 ) ;
#1274 = AXIS2_PLACEMENT_3D ( 'NONE', #403, #9959, #10010 ) ;
#1275 = DIRECTION ( 'NONE',  ( 0.000000000000000000, 0.000000000000000000, 1.000000000000000000 ) ) ;
#1276 = PRODUCT_DEFINITION ( 'UNKNOWN', '', #9579, #7173 ) ;
#1277 = LINE ( 'NONE', #10141, #1102 ) ;
#1278 = CARTESIAN_POINT ( 'NONE',  ( 11.30300220323380600, 6.000000000000000000, -12.00000000000000000 ) ) ;
#1279 = PLANE ( 'NONE',  #6189 ) ;
#1280 = LINE ( 'NONE', #4506, #5723 ) ;
#1281 = CARTESIAN_POINT ( 'NONE',  ( -0.6162731882459178134, -4.458484982038665834, 10.51605171672202133 ) ) ;
#1282 = CARTESIAN_POINT ( 'NONE',  ( -1.229367062500000163, -12.29022459553277002, -0.01041666734946308792 ) ) ;
#1283 = CARTESIAN_POINT ( 'NONE',  ( -3.279728542977953687, 3.411736077305369541, 12.30394828327797718 ) ) ;
#1284 = CARTESIAN_POINT ( 'NONE',  ( 1.229367062500000163, -13.00000000000000533, -0.2187500006827964583 ) ) ;
#1285 = AXIS2_PLACEMENT_3D ( 'NONE', #7974, #761, #8821 ) ;
#1286 = VERTEX_POINT ( 'NONE', #2412 ) ;
#1287 = DIRECTION ( 'NONE',  ( -0.000000000000000000, 1.000000000000000000, -0.000000000000000000 ) ) ;
#1288 = DIRECTION ( 'NONE',  ( -0.7071067811865335839, 0.000000000000000000, 0.7071067811865614505 ) ) ;
#1289 = CARTESIAN_POINT ( 'NONE',  ( 5.999999999999999112, 26.99999999999999289, -17.00000000000000000 ) ) ;
#1290 = CARTESIAN_POINT ( 'NONE',  ( -10.00000000000000000, 0.000000000000000000, 0.000000000000000000 ) ) ;
#1291 = ORIENTED_EDGE ( 'NONE', *, *, #984, .F. ) ;
#1292 = EDGE_CURVE ( 'NONE', #2419, #2608, #8875, .T. ) ;
#1293 = DIRECTION ( 'NONE',  ( 1.000000000000000000, 0.000000000000000000, 0.000000000000000000 ) ) ;
#1294 = PRESENTATION_STYLE_ASSIGNMENT (( #8606 ) ) ;
#1295 = CARTESIAN_POINT ( 'NONE',  ( -0.7401821875142701179, 4.673326407553649808, 2.379999999999999893 ) ) ;
#1296 = CARTESIAN_POINT ( 'NONE',  ( -0.6146835312500006365, -14.06466310670085562, -2.010416667349463005 ) ) ;
#1297 = ORIENTED_EDGE ( 'NONE', *, *, #1971, .T. ) ;
#1298 = ORIENTED_EDGE ( 'NONE', *, *, #1579, .T. ) ;
#1299 = CARTESIAN_POINT ( 'NONE',  ( 9.000000000000000000, 19.99999999999999645, 15.00000000000000000 ) ) ;
#1300 = LINE ( 'NONE', #5952, #9319 ) ;
#1301 = ORIENTED_EDGE ( 'NONE', *, *, #8334, .T. ) ;
#1302 = ADVANCED_FACE ( 'NONE', ( #9188 ), #9943, .F. ) ;
#1303 = CARTESIAN_POINT ( 'NONE',  ( -0.7727076532861475444, -5.446173322633804048, 7.716051716722023279 ) ) ;
#1304 = EDGE_CURVE ( 'NONE', #5208, #8945, #5835, .T. ) ;
#1305 = DIRECTION ( 'NONE',  ( 0.000000000000000000, -3.819167204710539130E-14, -1.000000000000000000 ) ) ;
#1306 = ORIENTED_EDGE ( 'NONE', *, *, #3124, .F. ) ;
#1307 = DIRECTION ( 'NONE',  ( -1.000000000000000000, -0.000000000000000000, 0.000000000000000000 ) ) ;
#1308 = ORIENTED_EDGE ( 'NONE', *, *, #5322, .T. ) ;
#1309 = FILL_AREA_STYLE_COLOUR ( '', #10249 ) ;
#1310 = EDGE_LOOP ( 'NONE', ( #2242, #7691, #7079, #9739 ) ) ;
#1311 = CARTESIAN_POINT ( 'NONE',  ( 15.00000000000000000, 19.99999999999999645, -5.999999999999999112 ) ) ;
#1312 = DIRECTION ( 'NONE',  ( 0.000000000000000000, 0.000000000000000000, 1.000000000000000000 ) ) ;
#1313 = ORIENTED_EDGE ( 'NONE', *, *, #8953, .T. ) ;
#1314 = ADVANCED_FACE ( 'NONE', ( #1926 ), #8447, .F. ) ;
#1315 = FACE_OUTER_BOUND ( 'NONE', #6062, .T. ) ;
#1316 = DIRECTION ( 'NONE',  ( -0.000000000000000000, -0.000000000000000000, -1.000000000000000000 ) ) ;
#1317 = CARTESIAN_POINT ( 'NONE',  ( 5.446173322633801384, 0.7727076532861675284, 7.683948283277975300 ) ) ;
#1318 = ORIENTED_EDGE ( 'NONE', *, *, #8066, .T. ) ;
#1319 = CARTESIAN_POINT ( 'NONE',  ( 5.999999999999999112, 26.99999999999999289, -14.00000000000000178 ) ) ;
#1320 = PLANE ( 'NONE',  #7513 ) ;
#1321 = CARTESIAN_POINT ( 'NONE',  ( 10.00000000000000000, 4.058600654062950674, -7.468451026206158083 ) ) ;
#1322 = DIRECTION ( 'NONE',  ( 0.000000000000000000, 0.000000000000000000, 1.000000000000000000 ) ) ;
#1323 = CARTESIAN_POINT ( 'NONE',  ( 0.000000000000000000, -27.00000000000000711, 0.000000000000000000 ) ) ;
#1324 = FACE_OUTER_BOUND ( 'NONE', #5872, .T. ) ;
#1325 = DIRECTION ( 'NONE',  ( -1.000000000000000000, -0.000000000000000000, -0.000000000000000000 ) ) ;
#1326 = CARTESIAN_POINT ( 'NONE',  ( 10.00000000000000000, 6.226349476952025341, 0.5315761383463611933 ) ) ;
#1327 = CARTESIAN_POINT ( 'NONE',  ( 4.173491630687861331, 2.231261971483781359, 9.536051716722020899 ) ) ;
#1328 = CARTESIAN_POINT ( 'NONE',  ( -0.6146835312500006365, -14.06466310670085562, 0.1145833326505365929 ) ) ;
#1329 = CARTESIAN_POINT ( 'NONE',  ( 5.195105386651219348, 2.542276634908100075, 10.34394828327797633 ) ) ;
#1330 = CARTESIAN_POINT ( 'NONE',  ( -1.229367062500000163, -13.70977540446723708, -1.427083334016129745 ) ) ;
#1331 = EDGE_LOOP ( 'NONE', ( #6517, #9789, #7113 ) ) ;
#1332 = DIRECTION ( 'NONE',  ( 1.000000000000000000, -0.000000000000000000, -0.000000000000000000 ) ) ;
#1333 = VECTOR ( 'NONE', #9587, 1000.000000000000000 ) ;
#1334 = LINE ( 'NONE', #10258, #2894 ) ;
#1335 = MECHANICAL_DESIGN_GEOMETRIC_PRESENTATION_REPRESENTATION (  '', ( #7777 ), #1870 ) ;
#1336 = CARTESIAN_POINT ( 'NONE',  ( -10.00000000000000000, 0.000000000000000000, 0.000000000000000000 ) ) ;
#1337 = FACE_OUTER_BOUND ( 'NONE', #8575, .T. ) ;
#1338 = ORIENTED_EDGE ( 'NONE', *, *, #6493, .T. ) ;
#1339 = VECTOR ( 'NONE', #8032, 1000.000000000000000 ) ;
#1340 = FACE_OUTER_BOUND ( 'NONE', #10401, .T. ) ;
#1341 = ADVANCED_FACE ( 'NONE', ( #6840 ), #10110, .T. ) ;
#1342 = DIRECTION ( 'NONE',  ( 0.000000000000000000, 0.000000000000000000, 1.000000000000000000 ) ) ;
#1343 = AXIS2_PLACEMENT_3D ( 'NONE', #2447, #59, #5 ) ;
#1344 = CARTESIAN_POINT ( 'NONE',  ( -0.6162731882459178134, -4.458484982038665834, 13.31605171672202204 ) ) ;
#1345 = VECTOR ( 'NONE', #7183, 1000.000000000000000 ) ;
#1346 = CARTESIAN_POINT ( 'NONE',  ( 1.229367062500000385, -12.29022459553277002, -1.302083334016129967 ) ) ;
#1347 = VERTEX_POINT ( 'NONE', #8075 ) ;
#1348 = EDGE_CURVE ( 'NONE', #8006, #5739, #10016, .T. ) ;
#1349 = VERTEX_POINT ( 'NONE', #6518 ) ;
#1350 = DIRECTION ( 'NONE',  ( 0.000000000000000000, 0.000000000000000000, -1.000000000000000000 ) ) ;
#1351 = AXIS2_PLACEMENT_3D ( 'NONE', #4874, #3979, #851 ) ;
#1352 = CARTESIAN_POINT ( 'NONE',  ( 19.29399126966725575, -7.750000000000000000, 0.000000000000000000 ) ) ;
#1353 = ORIENTED_EDGE ( 'NONE', *, *, #10459, .T. ) ;
#1354 = AXIS2_PLACEMENT_3D ( 'NONE', #3708, #3924, #6297 ) ;
#1355 = CARTESIAN_POINT ( 'NONE',  ( 4.940838830814703542, -2.417848759854246410, 9.956051716722022604 ) ) ;
#1356 = VERTEX_POINT ( 'NONE', #4034 ) ;
#1357 = PLANE ( 'NONE',  #1549 ) ;
#1358 = MECHANICAL_DESIGN_GEOMETRIC_PRESENTATION_REPRESENTATION (  '', ( #2040 ), #4064 ) ;
#1359 = ORIENTED_EDGE ( 'NONE', *, *, #6212, .F. ) ;
#1360 = VECTOR ( 'NONE', #3934, 1000.000000000000000 ) ;
#1361 = ORIENTED_EDGE ( 'NONE', *, *, #9230, .F. ) ;
#1362 = CIRCLE ( 'NONE', #3407, 3.000000000000000000 ) ;
#1363 = ADVANCED_FACE ( 'NONE', ( #2503, #753 ), #12, .F. ) ;
#1364 = LINE ( 'NONE', #1212, #4308 ) ;
#1365 = DIRECTION ( 'NONE',  ( 0.000000000000000000, 0.000000000000000000, 1.000000000000000000 ) ) ;
#1366 = AXIS2_PLACEMENT_3D ( 'NONE', #3051, #8669, #1515 ) ;
#1367 = ORIENTED_EDGE ( 'NONE', *, *, #7316, .T. ) ;
#1368 = DIRECTION ( 'NONE',  ( -1.000000000000000000, -0.000000000000000000, 0.000000000000000000 ) ) ;
#1369 = VECTOR ( 'NONE', #9141, 1000.000000000000000 ) ;
#1370 = DIRECTION ( 'NONE',  ( 0.000000000000000000, 0.000000000000000000, -1.000000000000000000 ) ) ;
#1371 = CARTESIAN_POINT ( 'NONE',  ( -4.023224611898323033, 4.155232146225737111, 6.703948283277976650 ) ) ;
#1372 = VERTEX_POINT ( 'NONE', #8916 ) ;
#1373 = DIRECTION ( 'NONE',  ( 1.000000000000000000, -0.000000000000000000, -0.000000000000000000 ) ) ;
#1374 = VECTOR ( 'NONE', #2108, 1000.000000000000227 ) ;
#1375 = DIRECTION ( 'NONE',  ( 0.000000000000000000, 0.000000000000000000, 1.000000000000000000 ) ) ;
#1376 = AXIS2_PLACEMENT_3D ( 'NONE', #1728, #978, #2674 ) ;
#1377 = EDGE_CURVE ( 'NONE', #9102, #6283, #3929, .T. ) ;
#1378 = DIRECTION ( 'NONE',  ( 0.000000000000000000, 0.000000000000000000, -1.000000000000000000 ) ) ;
#1379 = EDGE_CURVE ( 'NONE', #1396, #3111, #5667, .T. ) ;
#1380 = CARTESIAN_POINT ( 'NONE',  ( 0.000000000000000000, -13.00000000000000533, -3.000000000000000000 ) ) ;
#1381 = PLANE ( 'NONE',  #8477 ) ;
#1382 = DIRECTION ( 'NONE',  ( -1.000000000000000000, -0.000000000000000000, -0.000000000000000000 ) ) ;
#1383 = LINE ( 'NONE', #6299, #282 ) ;
#1384 = LINE ( 'NONE', #10246, #4886 ) ;
#1385 = CARTESIAN_POINT ( 'NONE',  ( 0.7401821875142697849, -4.673326407553650697, 6.579999999999999183 ) ) ;
#1386 = CARTESIAN_POINT ( 'NONE',  ( 0.6146835312499993043, -14.06466310670085562, -1.927083334016129967 ) ) ;
#1387 = CARTESIAN_POINT ( 'NONE',  ( -2.708615832122950096, -5.110351332421780413, 5.863948283277976792 ) ) ;
#1388 = EDGE_CURVE ( 'NONE', #3335, #7067, #7375, .T. ) ;
#1389 = PLANE ( 'NONE',  #397 ) ;
#1390 = VERTEX_POINT ( 'NONE', #3343 ) ;
#1391 = DIRECTION ( 'NONE',  ( 1.000000000000000000, 0.000000000000000000, 0.000000000000000000 ) ) ;
#1392 = CYLINDRICAL_SURFACE ( 'NONE', #10177, 8.500000000000000000 ) ;
#1393 = CARTESIAN_POINT ( 'NONE',  ( 0.4444353696672553311, 3.750000000000000000, -12.00000000000000000 ) ) ;
#1394 = CYLINDRICAL_SURFACE ( 'NONE', #8064, 8.500000000000000000 ) ;
#1395 = LINE ( 'NONE', #762, #4577 ) ;
#1396 = VERTEX_POINT ( 'NONE', #1553 ) ;
#1397 =( LENGTH_UNIT ( ) NAMED_UNIT ( * ) SI_UNIT ( .MILLI., .METRE. ) );
#1398 = LINE ( 'NONE', #6160, #5914 ) ;
#1399 = CARTESIAN_POINT ( 'NONE',  ( 0.7401821875142697849, -4.673326407553650697, 12.17999999999999439 ) ) ;
#1400 = CARTESIAN_POINT ( 'NONE',  ( 1.500000000000000000, -13.86602540378444459, -0.04166666666666684476 ) ) ;
#1401 = ORIENTED_EDGE ( 'NONE', *, *, #4133, .T. ) ;
#1402 = VERTEX_POINT ( 'NONE', #9022 ) ;
#1403 = CARTESIAN_POINT ( 'NONE',  ( 0.000000000000000000, 0.7390083445627224634, 1.279999999999999138 ) ) ;
#1404 = AXIS2_PLACEMENT_3D ( 'NONE', #4665, #5463, #4716 ) ;
#1405 = DIRECTION ( 'NONE',  ( -1.000000000000000000, -0.000000000000000000, -0.000000000000000000 ) ) ;
#1406 = ORIENTED_EDGE ( 'NONE', *, *, #874, .T. ) ;
#1407 = CARTESIAN_POINT ( 'NONE',  ( 0.9968613283357860011, -5.697241258616382531, 13.17605171672201969 ) ) ;
#1408 = DIRECTION ( 'NONE',  ( 0.3420201433256627732, 0.9396926207859105373, -0.000000000000000000 ) ) ;
#1409 = DIRECTION ( 'NONE',  ( -1.156482317317871478E-16, 1.000000000000000000, 0.000000000000000000 ) ) ;
#1410 = EDGE_LOOP ( 'NONE', ( #9527, #2908, #2491, #4743 ) ) ;
#1411 = CARTESIAN_POINT ( 'NONE',  ( 0.000000000000000000, 6.000000000000000000, -12.00000000000000000 ) ) ;
#1412 = CARTESIAN_POINT ( 'NONE',  ( 4.173491630687861331, 2.231261971483781359, 1.136051716722023208 ) ) ;
#1413 = EDGE_LOOP ( 'NONE', ( #3627, #3535, #1150, #6040 ) ) ;
#1414 = CIRCLE ( 'NONE', #1929, 2.000000000000000000 ) ;
#1415 = PRESENTATION_STYLE_ASSIGNMENT (( #5383 ) ) ;
#1416 = ORIENTED_EDGE ( 'NONE', *, *, #6395, .F. ) ;
#1417 = CARTESIAN_POINT ( 'NONE',  ( 13.83898384071655840, -10.02539999999999942, -12.00000000000000000 ) ) ;
#1418 = LINE ( 'NONE', #4644, #3557 ) ;
#1419 = ORIENTED_EDGE ( 'NONE', *, *, #7389, .T. ) ;
#1420 = LINE ( 'NONE', #3750, #9991 ) ;
#1421 = LINE ( 'NONE', #4762, #5297 ) ;
#1422 = CARTESIAN_POINT ( 'NONE',  ( 5.446173322633801384, 0.7727076532861675284, 4.883948283277976365 ) ) ;
#1423 = ORIENTED_EDGE ( 'NONE', *, *, #6274, .F. ) ;
#1424 = CARTESIAN_POINT ( 'NONE',  ( 1.060575238724907038E-16, -11.26794919243112680, -1.937500001365593416 ) ) ;
#1425 = EDGE_CURVE ( 'NONE', #9585, #6050, #867, .T. ) ;
#1426 = FACE_OUTER_BOUND ( 'NONE', #4809, .T. ) ;
#1427 =( BOUNDED_CURVE ( )  B_SPLINE_CURVE ( 2, ( #7646, #9285, #7539, #8545, #9987, #1871, #8394 ),
 .UNSPECIFIED., .F., .T. ) 
 B_SPLINE_CURVE_WITH_KNOTS ( ( 3, 2, 2, 3 ),
 ( 0.1666666666666666574, 0.1944444444444444475, 0.2222222222222222099, 0.2500000000000000000 ),
 .UNSPECIFIED. ) 
 CURVE ( )  GEOMETRIC_REPRESENTATION_ITEM ( )  RATIONAL_B_SPLINE_CURVE ( ( 1.000000000000000000, 0.8660254037844387076, 1.000000000000000000, 0.8660254037844387076, 1.000000000000000000, 0.8660254037844387076, 1.000000000000000000 ) ) 
 REPRESENTATION_ITEM ( '' )  );
#1428 = CARTESIAN_POINT ( 'NONE',  ( 1.530808498934183189E-16, 26.99999999999999289, -1.249999999999993339 ) ) ;
#1429 = CYLINDRICAL_SURFACE ( 'NONE', #3794, 3.000000000000000000 ) ;
#1430 = DIRECTION ( 'NONE',  ( 0.000000000000000000, 0.000000000000000000, 1.000000000000000000 ) ) ;
#1431 = CARTESIAN_POINT ( 'NONE',  ( -2.000000000000000000, -5.979767908488852868, 1.814490771706165351 ) ) ;
#1432 = DIRECTION ( 'NONE',  ( 5.204170427930421283E-15, 0.000000000000000000, 1.000000000000000000 ) ) ;
#1433 = VECTOR ( 'NONE', #6619, 1000.000000000000000 ) ;
#1434 = DIRECTION ( 'NONE',  ( -1.000000000000000000, -0.000000000000000000, -0.000000000000000000 ) ) ;
#1435 = CARTESIAN_POINT ( 'NONE',  ( -3.181980515339458027, -3.181980515339470905, 9.799999999999998934 ) ) ;
#1436 = EDGE_CURVE ( 'NONE', #1390, #6164, #3986, .T. ) ;
#1437 = EDGE_CURVE ( 'NONE', #4979, #4426, #6627, .T. ) ;
#1438 = CARTESIAN_POINT ( 'NONE',  ( 1.229367062500000385, -12.29022459553277002, -0.6770833340161300784 ) ) ;
#1439 = CARTESIAN_POINT ( 'NONE',  ( -5.195105386651219348, -2.542276634908102295, 11.74394828327797846 ) ) ;
#1440 = DIRECTION ( 'NONE',  ( 0.000000000000000000, 0.000000000000000000, -1.000000000000000000 ) ) ;
#1441 = VECTOR ( 'NONE', #6873, 1000.000000000000000 ) ;
#1442 = ORIENTED_EDGE ( 'NONE', *, *, #2860, .T. ) ;
#1443 = PRODUCT_CONTEXT ( 'NONE', #5988, 'mechanical' ) ;
#1444 = CARTESIAN_POINT ( 'NONE',  ( 0.000000000000000000, 6.000000000000000000, -12.00000000000000000 ) ) ;
#1445 = CARTESIAN_POINT ( 'NONE',  ( 11.00000000000000355, 0.000000000000000000, 0.000000000000000000 ) ) ;
#1446 = CARTESIAN_POINT ( 'NONE',  ( 1.272613240716556016, 6.025400000000000311, 0.000000000000000000 ) ) ;
#1447 = CARTESIAN_POINT ( 'NONE',  ( 0.000000000000000000, -19.00000000000000711, 0.000000000000000000 ) ) ;
#1448 = CARTESIAN_POINT ( 'NONE',  ( 0.000000000000000000, 0.000000000000000000, -4.000000000000000000 ) ) ;
#1449 = VERTEX_POINT ( 'NONE', #8386 ) ;
#1450 = EDGE_CURVE ( 'NONE', #7070, #4358, #9157, .T. ) ;
#1451 = VECTOR ( 'NONE', #8543, 1000.000000000000000 ) ;
#1452 = DIRECTION ( 'NONE',  ( 0.3420201433256627732, 0.9396926207859105373, -0.000000000000000000 ) ) ;
#1453 = AXIS2_PLACEMENT_3D ( 'NONE', #4245, #22, #5722 ) ;
#1454 = CARTESIAN_POINT ( 'NONE',  ( 0.7039550926810297371, 4.444597532678122853, 13.71999999999999886 ) ) ;
#1455 = UNCERTAINTY_MEASURE_WITH_UNIT (LENGTH_MEASURE( 1.000000000000000082E-05 ), #7334, 'distance_accuracy_value', 'NONE');
#1456 = CARTESIAN_POINT ( 'NONE',  ( -0.7499999999999997780, -11.70096189432334555, -0.8333333333333334814 ) ) ;
#1457 = ORIENTED_EDGE ( 'NONE', *, *, #4549, .T. ) ;
#1458 = AXIS2_PLACEMENT_3D ( 'NONE', #7318, #7211, #7096 ) ;
#1459 = VERTEX_POINT ( 'NONE', #9878 ) ;
#1460 = CIRCLE ( 'NONE', #3325, 6.248999999999999666 ) ;
#1461 = DIRECTION ( 'NONE',  ( -1.000000000000000000, -0.000000000000000000, -0.000000000000000000 ) ) ;
#1462 = DIRECTION ( 'NONE',  ( -0.3420201433256627732, -0.9396926207859105373, 0.000000000000000000 ) ) ;
#1463 = ORIENTED_EDGE ( 'NONE', *, *, #328, .T. ) ;
#1464 = CARTESIAN_POINT ( 'NONE',  ( 5.418398423912711870, 0.9480714621563913758, 6.876051716722023421 ) ) ;
#1465 = CARTESIAN_POINT ( 'NONE',  ( -2.607672531582950546E-16, -14.41955080893447416, 0.03124999931720332663 ) ) ;
#1466 = DIRECTION ( 'NONE',  ( -1.000000000000000000, -0.000000000000000000, -0.000000000000000000 ) ) ;
#1467 = ORIENTED_EDGE ( 'NONE', *, *, #1436, .F. ) ;
#1468 = LINE ( 'NONE', #7186, #3238 ) ;
#1469 = CARTESIAN_POINT ( 'NONE',  ( 4.940838830814703542, -2.417848759854246410, 9.956051716722022604 ) ) ;
#1470 = VERTEX_POINT ( 'NONE', #5190 ) ;
#1471 = VERTEX_POINT ( 'NONE', #8437 ) ;
#1472 = DIRECTION ( 'NONE',  ( -1.000000000000000000, -0.000000000000000000, -0.000000000000000000 ) ) ;
#1473 = DIRECTION ( 'NONE',  ( -1.000000000000000000, -0.000000000000000000, -0.000000000000000000 ) ) ;
#1474 = ORIENTED_EDGE ( 'NONE', *, *, #7964, .F. ) ;
#1475 = CARTESIAN_POINT ( 'NONE',  ( -5.999999999999999112, -27.00000000000000711, -14.00000000000000178 ) ) ;
#1476 = DIRECTION ( 'NONE',  ( -1.000000000000000000, -0.000000000000000000, -0.000000000000000000 ) ) ;
#1477 = CARTESIAN_POINT ( 'NONE',  ( -5.446173322633801384, -0.7727076532861678615, 0.6839482832779766319 ) ) ;
#1478 = VERTEX_POINT ( 'NONE', #2610 ) ;
#1479 = CARTESIAN_POINT ( 'NONE',  ( -1.229367062500000385, -13.70977540446723886, -2.427083334016129967 ) ) ;
#1480 = ADVANCED_FACE ( 'NONE', ( #7485 ), #5244, .F. ) ;
#1481 = DIRECTION ( 'NONE',  ( -0.000000000000000000, 1.000000000000000000, 0.000000000000000000 ) ) ;
#1482 = CARTESIAN_POINT ( 'NONE',  ( 10.00000000000000000, 0.000000000000000000, 0.000000000000000000 ) ) ;
#1483 = ORIENTED_EDGE ( 'NONE', *, *, #8967, .F. ) ;
#1484 = PRODUCT_DEFINITION_SHAPE ( 'NONE', 'NONE',  #7235 ) ;
#1485 = CARTESIAN_POINT ( 'NONE',  ( -2.000000000000001776, 2.449293598294706414E-16, -2.000000000000000000 ) ) ;
#1486 = ADVANCED_FACE ( 'NONE', ( #5139 ), #9931, .T. ) ;
#1487 = CARTESIAN_POINT ( 'NONE',  ( -1.500000000000000222, -13.00000000000000533, -2.250000000000000444 ) ) ;
#1488 = DIRECTION ( 'NONE',  ( 0.000000000000000000, 0.000000000000000000, -1.000000000000000000 ) ) ;
#1489 = CARTESIAN_POINT ( 'NONE',  ( 10.00000000000000000, 7.008469740302810891, -0.7425307242147085596 ) ) ;
#1490 = LINE ( 'NONE', #6360, #10314 ) ;
#1491 = CARTESIAN_POINT ( 'NONE',  ( 3.181980515339458471, 3.181980515339470461, 11.19999999999999751 ) ) ;
#1492 = CARTESIAN_POINT ( 'NONE',  ( 1.229367062500000385, -12.29022459553277002, -1.302083334016129967 ) ) ;
#1493 =( BOUNDED_CURVE ( )  B_SPLINE_CURVE ( 2, ( #6137, #3861, #7089, #7949, #9387, #2918, #687 ),
 .UNSPECIFIED., .F., .T. ) 
 B_SPLINE_CURVE_WITH_KNOTS ( ( 3, 2, 2, 3 ),
 ( 0.6666666666666666297, 0.6944444444444444198, 0.7222222222222222099, 0.7500000000000000000 ),
 .UNSPECIFIED. ) 
 CURVE ( )  GEOMETRIC_REPRESENTATION_ITEM ( )  RATIONAL_B_SPLINE_CURVE ( ( 1.000000000000000000, 0.8660254037844387076, 1.000000000000000000, 0.8660254037844387076, 1.000000000000000000, 0.8660254037844387076, 1.000000000000000000 ) ) 
 REPRESENTATION_ITEM ( '' )  );
#1494 = CARTESIAN_POINT ( 'NONE',  ( 0.9480714621563713917, 5.418398423912717199, 7.123948283277974802 ) ) ;
#1495 = CARTESIAN_POINT ( 'NONE',  ( 8.000000000000001776, -5.233522515400119701, 4.720195129223260899 ) ) ;
#1496 = ORIENTED_EDGE ( 'NONE', *, *, #1047, .F. ) ;
#1497 = APPLICATION_PROTOCOL_DEFINITION ( 'draft international standard', 'automotive_design', 1998, #3297 ) ;
#1498 = EDGE_CURVE ( 'NONE', #928, #4800, #4239, .T. ) ;
#1499 = CARTESIAN_POINT ( 'NONE',  ( 5.152728359536493663, 2.625446233515533745, 0.1399999999999999578 ) ) ;
#1500 = EDGE_CURVE ( 'NONE', #6214, #7824, #9077, .T. ) ;
#1501 = LINE ( 'NONE', #4094, #4493 ) ;
#1502 = ORIENTED_EDGE ( 'NONE', *, *, #4674, .F. ) ;
#1503 = LINE ( 'NONE', #3091, #5169 ) ;
#1504 = DIRECTION ( 'NONE',  ( -0.3420201433256627732, 0.9396926207859105373, 0.000000000000000000 ) ) ;
#1505 = EDGE_LOOP ( 'NONE', ( #2316, #3449, #2852, #4065 ) ) ;
#1506 = CARTESIAN_POINT ( 'NONE',  ( -0.7500000000000007772, -14.29903810567666156, -0.2291666680322604066 ) ) ;
#1507 = DIRECTION ( 'NONE',  ( -1.000000000000000000, -0.000000000000000000, -0.000000000000000000 ) ) ;
#1508 = CARTESIAN_POINT ( 'NONE',  ( -4.673326407553653361, 0.7401821875142517992, 7.419999999999998153 ) ) ;
#1509 = CARTESIAN_POINT ( 'NONE',  ( 0.7500000000000003331, -11.70096189432334732, -1.916666666666666741 ) ) ;
#1510 = AXIS2_PLACEMENT_3D ( 'NONE', #665, #1520, #3953 ) ;
#1511 = EDGE_LOOP ( 'NONE', ( #7554, #6393 ) ) ;
#1512 = EDGE_CURVE ( 'NONE', #9680, #4528, #7119, .T. ) ;
#1513 = ORIENTED_EDGE ( 'NONE', *, *, #7264, .T. ) ;
#1514 =( BOUNDED_CURVE ( )  B_SPLINE_CURVE ( 2, ( #2301, #5470, #7818, #3831, #9572, #2352, #10308 ),
 .UNSPECIFIED., .F., .T. ) 
 B_SPLINE_CURVE_WITH_KNOTS ( ( 3, 2, 2, 3 ),
 ( 0.4166666666666666297, 0.4444444444444443643, 0.4722222222222222099, 0.5000000000000000000 ),
 .UNSPECIFIED. ) 
 CURVE ( )  GEOMETRIC_REPRESENTATION_ITEM ( )  RATIONAL_B_SPLINE_CURVE ( ( 1.000000000000000222, 0.8660254037844384856, 1.000000000000000000, 0.8660254037844387076, 1.000000000000000000, 0.8660254037844387076, 1.000000000000000000 ) ) 
 REPRESENTATION_ITEM ( '' )  );
#1515 = DIRECTION ( 'NONE',  ( 1.000000000000000000, 0.000000000000000000, 0.000000000000000000 ) ) ;
#1516 = DIRECTION ( 'NONE',  ( 0.000000000000000000, -0.4999999999999992784, 0.8660254037844390407 ) ) ;
#1517 = EDGE_LOOP ( 'NONE', ( #6768, #8667, #1604, #8725 ) ) ;
#1518 = CARTESIAN_POINT ( 'NONE',  ( -0.8323763977770610722, 4.658724279160015413, 6.176051716722023244 ) ) ;
#1519 = CONICAL_SURFACE ( 'NONE', #7440, 1.249999999999997558, 1.029744258676650981 ) ;
#1520 = DIRECTION ( 'NONE',  ( 0.000000000000000000, 0.000000000000000000, 1.000000000000000000 ) ) ;
#1521 = PLANE ( 'NONE',  #10168 ) ;
#1522 = ORIENTED_EDGE ( 'NONE', *, *, #253, .T. ) ;
#1523 = CIRCLE ( 'NONE', #5067, 1.249999999999997558 ) ;
#1524 = DIRECTION ( 'NONE',  ( -1.000000000000000000, 0.000000000000000000, 0.000000000000000000 ) ) ;
#1525 = CARTESIAN_POINT ( 'NONE',  ( -2.576046737280769605, 4.860232935257343456, 14.43605171672202125 ) ) ;
#1526 = ORIENTED_EDGE ( 'NONE', *, *, #2218, .F. ) ;
#1527 = ADVANCED_FACE ( 'NONE', ( #7580 ), #323, .T. ) ;
#1528 = EDGE_LOOP ( 'NONE', ( #256, #6979, #7037, #4795 ) ) ;
#1529 = DIRECTION ( 'NONE',  ( 0.000000000000000000, 1.000000000000000000, 0.000000000000000000 ) ) ;
#1530 = AXIS2_PLACEMENT_3D ( 'NONE', #6853, #1832, #8358 ) ;
#1531 = CARTESIAN_POINT ( 'NONE',  ( 10.00000000000000000, -1.471047635026825784, -6.892461014225975013 ) ) ;
#1532 = EDGE_LOOP ( 'NONE', ( #6973, #5382, #7121, #4739 ) ) ;
#1533 = FACE_OUTER_BOUND ( 'NONE', #2534, .T. ) ;
#1534 = LINE ( 'NONE', #8004, #6645 ) ;
#1535 = CARTESIAN_POINT ( 'NONE',  ( 2.708615832122949652, 5.110351332421781301, 7.263948283277976259 ) ) ;
#1536 = ORIENTED_EDGE ( 'NONE', *, *, #808, .F. ) ;
#1537 = VECTOR ( 'NONE', #10492, 1000.000000000000000 ) ;
#1538 = CARTESIAN_POINT ( 'NONE',  ( 1.500000000000000000, -13.86602540378444459, 0.3958333319677397322 ) ) ;
#1539 = AXIS2_PLACEMENT_3D ( 'NONE', #10294, #6141, #1430 ) ;
#1540 = DIRECTION ( 'NONE',  ( -1.000000000000000000, -0.000000000000000000, 0.000000000000000000 ) ) ;
#1541 = COLOUR_RGB ( '', 0.66274510, 0.83137255, 0.94901961) ;
#1542 = ORIENTED_EDGE ( 'NONE', *, *, #8446, .T. ) ;
#1543 = CIRCLE ( 'NONE', #871, 1.500000000000000222 ) ;
#1544 = CARTESIAN_POINT ( 'NONE',  ( 1.499999999999999778, -13.86602540378444637, -0.6041666680322602678 ) ) ;
#1545 = AXIS2_PLACEMENT_3D ( 'NONE', #883, #8149, #6541 ) ;
#1546 = DIRECTION ( 'NONE',  ( 0.000000000000000000, 0.000000000000000000, 1.000000000000000000 ) ) ;
#1547 = DIRECTION ( 'NONE',  ( 0.000000000000000000, 0.000000000000000000, -1.000000000000000000 ) ) ;
#1548 = LINE ( 'NONE', #2337, #4328 ) ;
#1549 = AXIS2_PLACEMENT_3D ( 'NONE', #10072, #2060, #5285 ) ;
#1550 = CARTESIAN_POINT ( 'NONE',  ( 22.43558391966725907, -7.750000000000000000, -12.00000000000000000 ) ) ;
#1551 = CARTESIAN_POINT ( 'NONE',  ( -2.148092372876330813, -4.215868657802593233, 9.659999999999994813 ) ) ;
#1552 = ORIENTED_EDGE ( 'NONE', *, *, #4165, .T. ) ;
#1553 = CARTESIAN_POINT ( 'NONE',  ( 25.00000000000000000, 0.000000000000000000, -2.000000000000000000 ) ) ;
#1554 = VECTOR ( 'NONE', #5686, 1000.000000000000000 ) ;
#1555 = ADVANCED_FACE ( 'NONE', ( #3551 ), #225, .T. ) ;
#1556 = CARTESIAN_POINT ( 'NONE',  ( 4.860232935257354114, -2.576046737280751842, 5.163948283277975726 ) ) ;
#1557 = DIRECTION ( 'NONE',  ( 0.000000000000000000, -0.000000000000000000, 1.000000000000000000 ) ) ;
#1558 = ORIENTED_EDGE ( 'NONE', *, *, #382, .T. ) ;
#1559 = CARTESIAN_POINT ( 'NONE',  ( -4.089228379062038066, 4.089228379062022078, 2.099999999999999645 ) ) ;
#1560 = CARTESIAN_POINT ( 'NONE',  ( 0.000000000000000000, -13.00000000000000533, 2.000000000000000000 ) ) ;
#1561 = ORIENTED_EDGE ( 'NONE', *, *, #6420, .F. ) ;
#1562 = CARTESIAN_POINT ( 'NONE',  ( -10.00000000000000000, 0.000000000000000000, 0.000000000000000000 ) ) ;
#1563 = LINE ( 'NONE', #4787, #2890 ) ;
#1564 = FACE_OUTER_BOUND ( 'NONE', #2785, .T. ) ;
#1565 =( NAMED_UNIT ( * ) SI_UNIT ( $, .STERADIAN. ) SOLID_ANGLE_UNIT ( ) );
#1566 = CARTESIAN_POINT ( 'NONE',  ( 12.99999999999999645, 19.99999999999999645, -5.999999999999999112 ) ) ;
#1567 = ADVANCED_FACE ( 'NONE', ( #2760 ), #5974, .T. ) ;
#1568 = CARTESIAN_POINT ( 'NONE',  ( -4.009529358847660596, 2.042957248827953265, 7.559999999999998721 ) ) ;
#1569 = UNCERTAINTY_MEASURE_WITH_UNIT (LENGTH_MEASURE( 1.000000000000000082E-05 ), #5698, 'distance_accuracy_value', 'NONE');
#1570 = CARTESIAN_POINT ( 'NONE',  ( 1.060575238724907038E-16, -11.26794919243112680, -1.375000000000000222 ) ) ;
#1571 = ORIENTED_EDGE ( 'NONE', *, *, #5320, .T. ) ;
#1572 = ORIENTED_EDGE ( 'NONE', *, *, #8813, .F. ) ;
#1573 = LINE ( 'NONE', #8774, #3569 ) ;
#1574 = LINE ( 'NONE', #3841, #2550 ) ;
#1575 = ORIENTED_EDGE ( 'NONE', *, *, #6363, .T. ) ;
#1576 = CARTESIAN_POINT ( 'NONE',  ( -1.500000000000000222, -13.00000000000000533, -3.000000000000000000 ) ) ;
#1577 = FACE_BOUND ( 'NONE', #5153, .T. ) ;
#1578 = ORIENTED_EDGE ( 'NONE', *, *, #9879, .T. ) ;
#1579 = EDGE_CURVE ( 'NONE', #8329, #6538, #9123, .T. ) ;
#1580 = EDGE_CURVE ( 'NONE', #4280, #2958, #9229, .T. ) ;
#1581 = CARTESIAN_POINT ( 'NONE',  ( 10.00000000000000000, 0.000000000000000000, 0.000000000000000000 ) ) ;
#1582 = CARTESIAN_POINT ( 'NONE',  ( -3.411736077305382420, 3.279728542977939476, 3.096051716722023617 ) ) ;
#1583 = PRODUCT_DEFINITION_SHAPE ( 'NONE', 'NONE',  #10500 ) ;
#1584 = VERTEX_POINT ( 'NONE', #7530 ) ;
#1585 = AXIS2_PLACEMENT_3D ( 'NONE', #5606, #10454, #8060 ) ;
#1586 = LINE ( 'NONE', #731, #97 ) ;
#1587 = DIRECTION ( 'NONE',  ( -0.000000000000000000, -0.000000000000000000, 1.000000000000000000 ) ) ;
#1588 = ORIENTED_EDGE ( 'NONE', *, *, #2160, .F. ) ;
#1589 = CARTESIAN_POINT ( 'NONE',  ( 2.625446233515515537, 5.152728359536502545, 8.259999999999999787 ) ) ;
#1590 = LINE ( 'NONE', #9652, #7504 ) ;
#1591 = CARTESIAN_POINT ( 'NONE',  ( -5.711843387010018702, 0.9046671180729746187, 4.620000000000000107 ) ) ;
#1592 = VERTEX_POINT ( 'NONE', #3502 ) ;
#1593 = ADVANCED_FACE ( 'NONE', ( #4189 ), #1969, .F. ) ;
#1594 = CARTESIAN_POINT ( 'NONE',  ( 0.7499999999999991118, -14.29903810567666333, -0.1458333346989267310 ) ) ;
#1595 = AXIS2_PLACEMENT_3D ( 'NONE', #5090, #2660, #3294 ) ;
#1596 =( NAMED_UNIT ( * ) PLANE_ANGLE_UNIT ( ) SI_UNIT ( $, .RADIAN. ) );
#1597 = VERTEX_POINT ( 'NONE', #6830 ) ;
#1598 = LINE ( 'NONE', #744, #5152 ) ;
#1599 = LINE ( 'NONE', #4873, #8156 ) ;
#1600 = CARTESIAN_POINT ( 'NONE',  ( 1.499999999999999778, -13.86602540378444637, -2.041666666666666963 ) ) ;
#1601 = CARTESIAN_POINT ( 'NONE',  ( -26.99999999999998934, -32.00000000000000000, -5.999999999999999112 ) ) ;
#1602 = DIRECTION ( 'NONE',  ( -1.000000000000000000, -0.000000000000000000, -0.000000000000000000 ) ) ;
#1603 = CARTESIAN_POINT ( 'NONE',  ( 0.7039550926810297371, 4.444597532678122853, 8.119999999999999218 ) ) ;
#1604 = ORIENTED_EDGE ( 'NONE', *, *, #5366, .F. ) ;
#1605 = CARTESIAN_POINT ( 'NONE',  ( -1.229367062500000163, -13.00000000000000533, -0.09375000068279679133 ) ) ;
#1606 = CARTESIAN_POINT ( 'NONE',  ( -4.900535883036028828, 2.496947748567499126, 7.559999999999998721 ) ) ;
#1607 = DIRECTION ( 'NONE',  ( 0.000000000000000000, 1.000000000000000000, -1.320393690296331133E-15 ) ) ;
#1608 = APPLICATION_PROTOCOL_DEFINITION ( 'draft international standard', 'automotive_design', 1998, #8714 ) ;
#1609 = CARTESIAN_POINT ( 'NONE',  ( -0.9046671180729962680, 5.711843387010016926, 2.379999999999999893 ) ) ;
#1610 = CARTESIAN_POINT ( 'NONE',  ( 0.000000000000000000, 26.99999999999999289, 0.000000000000000000 ) ) ;
#1611 = DIRECTION ( 'NONE',  ( 0.000000000000000000, -0.000000000000000000, 1.000000000000000000 ) ) ;
#1612 = CARTESIAN_POINT ( 'NONE',  ( 7.401486830834375884E-15, -31.99999999999999289, 0.000000000000000000 ) ) ;
#1613 = EDGE_CURVE ( 'NONE', #7025, #5618, #2385, .T. ) ;
#1614 = DIRECTION ( 'NONE',  ( -1.000000000000000000, 0.000000000000000000, 0.000000000000000000 ) ) ;
#1615 = CARTESIAN_POINT ( 'NONE',  ( 25.00000000000000000, -7.750000000000000000, -12.00000000000000000 ) ) ;
#1616 = DIRECTION ( 'NONE',  ( -1.000000000000000000, -1.156482317317871478E-16, -5.694029147589358720E-15 ) ) ;
#1617 = CIRCLE ( 'NONE', #9576, 1.500000000000000222 ) ;
#1618 = CARTESIAN_POINT ( 'NONE',  ( 4.215868657802586128, 2.148092372876346801, 8.539999999999999147 ) ) ;
#1619 = CARTESIAN_POINT ( 'NONE',  ( 1.500000000000000222, -13.00000000000000533, -1.000000000000000000 ) ) ;
#1620 = ORIENTED_EDGE ( 'NONE', *, *, #8293, .F. ) ;
#1621 = ORIENTED_EDGE ( 'NONE', *, *, #7477, .T. ) ;
#1622 = DIRECTION ( 'NONE',  ( 0.000000000000000000, 0.000000000000000000, -1.000000000000000000 ) ) ;
#1623 = AXIS2_PLACEMENT_3D ( 'NONE', #1311, #3909, #3796 ) ;
#1624 = EDGE_CURVE ( 'NONE', #909, #2796, #167, .T. ) ;
#1625 =( NAMED_UNIT ( * ) PLANE_ANGLE_UNIT ( ) SI_UNIT ( $, .RADIAN. ) );
#1626 = ORIENTED_EDGE ( 'NONE', *, *, #4152, .F. ) ;
#1627 = CIRCLE ( 'NONE', #9936, 3.000000000000000000 ) ;
#1628 = CARTESIAN_POINT ( 'NONE',  ( 16.15239861966725599, 3.750000000000000000, 0.000000000000000000 ) ) ;
#1629 = DIRECTION ( 'NONE',  ( -1.000000000000000000, -0.000000000000000000, -0.000000000000000000 ) ) ;
#1630 = ORIENTED_EDGE ( 'NONE', *, *, #9453, .F. ) ;
#1631 = CARTESIAN_POINT ( 'NONE',  ( -5.726445515403654873, 0.8124729078101847746, 14.01605171672202310 ) ) ;
#1632 = CIRCLE ( 'NONE', #280, 3.000000000000000000 ) ;
#1633 = ORIENTED_EDGE ( 'NONE', *, *, #8504, .T. ) ;
#1634 = ORIENTED_EDGE ( 'NONE', *, *, #9019, .F. ) ;
#1635 = EDGE_CURVE ( 'NONE', #1592, #6214, #5448, .T. ) ;
#1636 = CARTESIAN_POINT ( 'NONE',  ( 0.000000000000000000, -19.00000000000000711, 0.000000000000000000 ) ) ;
#1637 = EDGE_CURVE ( 'NONE', #371, #5056, #4240, .T. ) ;
#1638 = CARTESIAN_POINT ( 'NONE',  ( 27.00000000000001066, -34.99999999999999289, 5.999999999999999112 ) ) ;
#1639 = VERTEX_POINT ( 'NONE', #6985 ) ;
#1640 = CARTESIAN_POINT ( 'NONE',  ( 4.089228379062037178, -4.089228379062022967, 6.299999999999999822 ) ) ;
#1641 = CARTESIAN_POINT ( 'NONE',  ( 8.000000000000001776, 5.471841788314748989, -3.018103451449677621 ) ) ;
#1642 = CARTESIAN_POINT ( 'NONE',  ( 4.860232935257354114, -2.576046737280751842, 10.76394828327797626 ) ) ;
#1643 = VERTEX_POINT ( 'NONE', #2969 ) ;
#1644 = CARTESIAN_POINT ( 'NONE',  ( -0.7499999999999997780, -11.70096189432334555, -1.395833334698926897 ) ) ;
#1645 = VERTEX_POINT ( 'NONE', #7039 ) ;
#1646 = EDGE_CURVE ( 'NONE', #10253, #5539, #7742, .T. ) ;
#1647 = CARTESIAN_POINT ( 'NONE',  ( 0.000000000000000000, 0.000000000000000000, 6.999999999999999112 ) ) ;
#1648 = CARTESIAN_POINT ( 'NONE',  ( -2.500000000000000000, 0.000000000000000000, -4.000000000000000000 ) ) ;
#1649 = CARTESIAN_POINT ( 'NONE',  ( 17.58618750323380908, -10.00000000000000000, -12.00000000000000000 ) ) ;
#1650 = LINE ( 'NONE', #802, #5733 ) ;
#1651 = LINE ( 'NONE', #4710, #4829 ) ;
#1652 = CARTESIAN_POINT ( 'NONE',  ( 4.258245684917310037, 2.064922774268912686, 4.743948283277974909 ) ) ;
#1653 = ORIENTED_EDGE ( 'NONE', *, *, #567, .F. ) ;
#1654 = DIRECTION ( 'NONE',  ( -1.000000000000000000, 0.000000000000000000, 0.000000000000000000 ) ) ;
#1655 = CARTESIAN_POINT ( 'NONE',  ( 0.8603895577212593571, 5.432285873273261068, 8.119999999999999218 ) ) ;
#1656 = LINE ( 'NONE', #9933, #5135 ) ;
#1657 = ITEM_DEFINED_TRANSFORMATION ( 'NONE', 'NONE', #9066,  #2101 ) ;
#1658 = EDGE_CURVE ( 'NONE', #618, #928, #5394, .T. ) ;
#1659 = DIRECTION ( 'NONE',  ( -1.000000000000000000, -0.000000000000000000, 0.000000000000000000 ) ) ;
#1660 = PLANE ( 'NONE',  #3811 ) ;
#1661 = CARTESIAN_POINT ( 'NONE',  ( 14.43535000928344481, -10.02539999999999942, -12.00000000000000000 ) ) ;
#1662 = LINE ( 'NONE', #7276, #3571 ) ;
#1663 = PRODUCT_DEFINITION_SHAPE ( 'NONE', 'NONE',  #10502 ) ;
#1664 = DIRECTION ( 'NONE',  ( -0.3420201433256627732, -0.9396926207859105373, 0.000000000000000000 ) ) ;
#1665 = LINE ( 'NONE', #6477, #5589 ) ;
#1666 = CARTESIAN_POINT ( 'NONE',  ( 0.6479879772514793856, -4.687928535947285091, 5.583948283277975655 ) ) ;
#1667 = UNCERTAINTY_MEASURE_WITH_UNIT (LENGTH_MEASURE( 1.000000000000000082E-05 ), #10273, 'distance_accuracy_value', 'NONE');
#1668 = CARTESIAN_POINT ( 'NONE',  ( -1.229367062500000163, -13.00000000000000533, -2.468750000682796486 ) ) ;
#1669 = ORIENTED_EDGE ( 'NONE', *, *, #4036, .F. ) ;
#1670 = ORIENTED_EDGE ( 'NONE', *, *, #287, .F. ) ;
#1671 = CARTESIAN_POINT ( 'NONE',  ( -10.00000000000000000, 0.000000000000000000, 0.000000000000000000 ) ) ;
#1672 = FACE_OUTER_BOUND ( 'NONE', #8195, .T. ) ;
#1673 = EDGE_CURVE ( 'NONE', #9650, #7351, #6237, .T. ) ;
#1674 = EDGE_LOOP ( 'NONE', ( #7911, #6354, #704, #39, #1693 ) ) ;
#1675 = CARTESIAN_POINT ( 'NONE',  ( -0.7401821875142703400, 4.673326407553649808, 5.179999999999999716 ) ) ;
#1676 =( REPRESENTATION_RELATIONSHIP ('NONE','NONE', #5100, #6499 ) REPRESENTATION_RELATIONSHIP_WITH_TRANSFORMATION ( #1657 )SHAPE_REPRESENTATION_RELATIONSHIP( ) );
#1677 = CARTESIAN_POINT ( 'NONE',  ( 0.000000000000000000, 0.000000000000000000, -14.00000000000000178 ) ) ;
#1678 = EDGE_LOOP ( 'NONE', ( #3431, #3738, #89, #4935 ) ) ;
#1679 = CIRCLE ( 'NONE', #3204, 8.500000000000000000 ) ;
#1680 = CARTESIAN_POINT ( 'NONE',  ( 2.122056237541221524, -3.969226411068978777, 7.436051716722023031 ) ) ;
#1681 = EDGE_CURVE ( 'NONE', #4156, #3105, #9337, .T. ) ;
#1682 = ORIENTED_EDGE ( 'NONE', *, *, #3635, .F. ) ;
#1683 =( LENGTH_UNIT ( ) NAMED_UNIT ( * ) SI_UNIT ( .MILLI., .METRE. ) );
#1684 = ORIENTED_EDGE ( 'NONE', *, *, #552, .T. ) ;
#1685 = DIRECTION ( 'NONE',  ( 0.000000000000000000, 1.000000000000000000, -1.224646799147353207E-16 ) ) ;
#1686 = VECTOR ( 'NONE', #2465, 1000.000000000000000 ) ;
#1687 = CARTESIAN_POINT ( 'NONE',  ( 18.40512053033274853, -7.750000000000000000, -12.00000000000000000 ) ) ;
#1688 = ORIENTED_EDGE ( 'NONE', *, *, #1247, .F. ) ;
#1689 = VECTOR ( 'NONE', #1157, 1000.000000000000000 ) ;
#1690 = CARTESIAN_POINT ( 'NONE',  ( 5.152728359536493663, 2.625446233515533745, 0.1399999999999999856 ) ) ;
#1691 = FACE_OUTER_BOUND ( 'NONE', #2438, .T. ) ;
#1692 = CARTESIAN_POINT ( 'NONE',  ( -2.625446233515515981, -5.152728359536500768, 4.059999999999999609 ) ) ;
#1693 = ORIENTED_EDGE ( 'NONE', *, *, #7532, .T. ) ;
#1694 = CLOSED_SHELL ( 'NONE', ( #8951, #7126, #899, #6555, #3591, #5158, #1826, #7597, #6877, #2925, #6151, #9389, #5773, #7219, #4790, #2772, #10485, #7051, #1245, #8375, #10268, #69, #7794, #9093, #94, #4327, #5644 ) ) ;
#1695 = CARTESIAN_POINT ( 'NONE',  ( -0.7500000000000007772, -14.29903810567666156, 0.2708333319677396211 ) ) ;
#1696 = AXIS2_PLACEMENT_3D ( 'NONE', #7628, #3647, #9380 ) ;
#1697 = VERTEX_POINT ( 'NONE', #1319 ) ;
#1698 = DIRECTION ( 'NONE',  ( 0.000000000000000000, 0.000000000000000000, 1.000000000000000000 ) ) ;
#1699 = FACE_OUTER_BOUND ( 'NONE', #7725, .T. ) ;
#1700 = CARTESIAN_POINT ( 'NONE',  ( 16.15239861966725599, -7.750000000000000000, 0.000000000000000000 ) ) ;
#1701 = CARTESIAN_POINT ( 'NONE',  ( 30.00000000000001066, 0.000000000000000000, 0.000000000000000000 ) ) ;
#1702 = CIRCLE ( 'NONE', #6762, 2.000000000000000000 ) ;
#1703 = DIRECTION ( 'NONE',  ( 0.000000000000000000, 0.000000000000000000, -1.000000000000000000 ) ) ;
#1704 = CARTESIAN_POINT ( 'NONE',  ( -0.7916369971161423269, -4.430710083317576320, 2.923948283277976401 ) ) ;
#1705 = EDGE_LOOP ( 'NONE', ( #9011, #6484, #2571, #8572 ) ) ;
#1706 = AXIS2_PLACEMENT_3D ( 'NONE', #9359, #603, #2095 ) ;
#1707 = CARTESIAN_POINT ( 'NONE',  ( 25.00000000000000000, 0.000000000000000000, -2.000000000000000000 ) ) ;
#1708 = EDGE_CURVE ( 'NONE', #3161, #7840, #1220, .T. ) ;
#1709 = EDGE_CURVE ( 'NONE', #7874, #8403, #4544, .T. ) ;
#1710 = CARTESIAN_POINT ( 'NONE',  ( -5.432285873273256627, -0.8603895577212797852, 1.679999999999999938 ) ) ;
#1711 = LINE ( 'NONE', #1866, #9206 ) ;
#1712 = AXIS2_PLACEMENT_3D ( 'NONE', #88, #3363, #9095 ) ;
#1713 = CONTEXT_DEPENDENT_SHAPE_REPRESENTATION ( #1272, #313 ) ;
#1714 = CARTESIAN_POINT ( 'NONE',  ( 5.432285873273257515, 0.8603895577212793411, 5.879999999999999893 ) ) ;
#1715 = AXIS2_PLACEMENT_3D ( 'NONE', #10086, #6776, #2813 ) ;
#1716 = CARTESIAN_POINT ( 'NONE',  ( 1.500000000000000222, -13.00000000000000533, -1.562500001365593416 ) ) ;
#1717 = FACE_BOUND ( 'NONE', #2962, .T. ) ;
#1718 = PLANE ( 'NONE',  #6271 ) ;
#1719 = CIRCLE ( 'NONE', #8323, 3.000000000000000000 ) ;
#1720 = CARTESIAN_POINT ( 'NONE',  ( 23.26376179071655770, 6.025400000000000311, 0.000000000000000000 ) ) ;
#1721 = CARTESIAN_POINT ( 'NONE',  ( -3.119207202478379681, -3.244753828200550139, 5.196051716722022817 ) ) ;
#1722 = AXIS2_PLACEMENT_3D ( 'NONE', #8083, #1913, #5134 ) ;
#1723 = EDGE_CURVE ( 'NONE', #1757, #7886, #4598, .T. ) ;
#1724 = CARTESIAN_POINT ( 'NONE',  ( 3.279728542977952799, -3.411736077305369541, 8.103948283277974340 ) ) ;
#1725 = DIRECTION ( 'NONE',  ( -1.000000000000000000, -0.000000000000000000, -0.000000000000000000 ) ) ;
#1726 = ORIENTED_EDGE ( 'NONE', *, *, #21, .F. ) ;
#1727 = ORIENTED_EDGE ( 'NONE', *, *, #3755, .T. ) ;
#1728 = CARTESIAN_POINT ( 'NONE',  ( -2.000000000000000000, 0.000000000000000000, 0.000000000000000000 ) ) ;
#1729 = DIRECTION ( 'NONE',  ( -1.000000000000000000, -0.000000000000000000, -0.000000000000000000 ) ) ;
#1730 = VERTEX_POINT ( 'NONE', #5346 ) ;
#1731 = CARTESIAN_POINT ( 'NONE',  ( -0.7401821875142703400, 4.673326407553649808, 2.379999999999999893 ) ) ;
#1732 = DIRECTION ( 'NONE',  ( 0.000000000000000000, 0.000000000000000000, 1.000000000000000000 ) ) ;
#1733 = ORIENTED_EDGE ( 'NONE', *, *, #2258, .T. ) ;
#1734 = CARTESIAN_POINT ( 'NONE',  ( -3.119207202478379681, -3.244753828200550139, 5.196051716722022817 ) ) ;
#1735 = CARTESIAN_POINT ( 'NONE',  ( -1.229367062500000385, -13.70977540446723886, -2.552083334016129967 ) ) ;
#1736 = EDGE_LOOP ( 'NONE', ( #10338, #679, #7987, #4069 ) ) ;
#1737 = VERTEX_POINT ( 'NONE', #5296 ) ;
#1738 = CARTESIAN_POINT ( 'NONE',  ( 19.29399126966725575, -7.750000000000000000, -12.00000000000000000 ) ) ;
#1739 = SURFACE_SIDE_STYLE ('',( #4268 ) ) ;
#1740 = ORIENTED_EDGE ( 'NONE', *, *, #4922, .F. ) ;
#1741 = CARTESIAN_POINT ( 'NONE',  ( 0.8603895577212593571, 5.432285873273261068, 5.319999999999999396 ) ) ;
#1742 = CARTESIAN_POINT ( 'NONE',  ( 0.9046671180729951578, -5.711843387010016926, 0.9799999999999997602 ) ) ;
#1743 = CARTESIAN_POINT ( 'NONE',  ( 5.432285873273257515, 0.8603895577212793411, 0.2799999999999999156 ) ) ;
#1744 = VERTEX_POINT ( 'NONE', #9443 ) ;
#1745 = CARTESIAN_POINT ( 'NONE',  ( 1.229367062500000385, -12.29022459553277002, -0.1770833340161300229 ) ) ;
#1746 = AXIS2_PLACEMENT_3D ( 'NONE', #50, #737, #6289 ) ;
#1747 = VERTEX_POINT ( 'NONE', #3806 ) ;
#1748 = LINE ( 'NONE', #955, #8553 ) ;
#1749 = CARTESIAN_POINT ( 'NONE',  ( -5.999999999999999112, -27.00000000000000711, 3.000000000000000000 ) ) ;
#1750 = CARTESIAN_POINT ( 'NONE',  ( 1.500000000000000222, -13.00000000000000533, -1.062500001365593416 ) ) ;
#1751 = EDGE_LOOP ( 'NONE', ( #7175, #733, #2152, #6231 ) ) ;
#1752 = DIRECTION ( 'NONE',  ( 0.000000000000000000, 0.000000000000000000, 1.000000000000000000 ) ) ;
#1753 = EDGE_CURVE ( 'NONE', #2266, #946, #4443, .T. ) ;
#1754 = AXIS2_PLACEMENT_3D ( 'NONE', #7857, #8866, #1557 ) ;
#1755 = CARTESIAN_POINT ( 'NONE',  ( -0.6146835312500006365, -14.06466310670085562, -2.510416667349463005 ) ) ;
#1756 = CARTESIAN_POINT ( 'NONE',  ( 1.963858260114715870, -4.049832306626327316, -0.1560517167220233370 ) ) ;
#1757 = VERTEX_POINT ( 'NONE', #6883 ) ;
#1758 = CARTESIAN_POINT ( 'NONE',  ( 10.00000000000000000, 0.000000000000000000, 0.000000000000000000 ) ) ;
#1759 = CARTESIAN_POINT ( 'NONE',  ( -2.625446233515515981, -5.152728359536500768, 4.059999999999999609 ) ) ;
#1760 = CARTESIAN_POINT ( 'NONE',  ( -2.143395387092215042E-15, 18.24892422621553933, 0.000000000000000000 ) ) ;
#1761 = ITEM_DEFINED_TRANSFORMATION ( 'NONE', 'NONE', #9406,  #2101 ) ;
#1762 = AXIS2_PLACEMENT_3D ( 'NONE', #4501, #7745, #326 ) ;
#1763 = CARTESIAN_POINT ( 'NONE',  ( 2.625446233515515093, 5.152728359536503433, 8.259999999999999787 ) ) ;
#1764 = DIRECTION ( 'NONE',  ( -1.000000000000000000, -0.000000000000000000, 0.000000000000000000 ) ) ;
#1765 = ADVANCED_FACE ( 'NONE', ( #10189 ), #7590, .T. ) ;
#1766 = DIRECTION ( 'NONE',  ( 0.000000000000000000, 0.000000000000000000, 1.000000000000000000 ) ) ;
#1767 = EDGE_CURVE ( 'NONE', #2958, #9757, #952, .T. ) ;
#1768 = CARTESIAN_POINT ( 'NONE',  ( 12.12193523033274545, 3.750000000000000000, -12.00000000000000000 ) ) ;
#1769 = CARTESIAN_POINT ( 'NONE',  ( 3.119207202478379681, 3.244753828200549695, 3.796051716722023350 ) ) ;
#1770 = VECTOR ( 'NONE', #6028, 1000.000000000000000 ) ;
#1771 = CARTESIAN_POINT ( 'NONE',  ( -3.969226411068985882, 2.122056237541205537, 9.363948283277975904 ) ) ;
#1772 = CARTESIAN_POINT ( 'NONE',  ( 15.00000000000000000, 19.99999999999999645, -9.000000000000000000 ) ) ;
#1773 = ORIENTED_EDGE ( 'NONE', *, *, #7796, .T. ) ;
#1774 =( BOUNDED_CURVE ( )  B_SPLINE_CURVE ( 2, ( #10278, #3847, #7732, #2955, #3007, #7883, #416 ),
 .UNSPECIFIED., .F., .T. ) 
 B_SPLINE_CURVE_WITH_KNOTS ( ( 3, 2, 2, 3 ),
 ( 0.3333333333333333148, 0.3611111111111111049, 0.3888888888888888395, 0.4166666666666666297 ),
 .UNSPECIFIED. ) 
 CURVE ( )  GEOMETRIC_REPRESENTATION_ITEM ( )  RATIONAL_B_SPLINE_CURVE ( ( 1.000000000000000000, 0.8660254037844387076, 1.000000000000000000, 0.8660254037844387076, 1.000000000000000000, 0.8660254037844389297, 0.9999999999999997780 ) ) 
 REPRESENTATION_ITEM ( '' )  );
#1775 = CARTESIAN_POINT ( 'NONE',  ( 5.418398423912711870, 0.9480714621563913758, 6.876051716722023421 ) ) ;
#1776 = STYLED_ITEM ( 'NONE', ( #2430 ), #4603 ) ;
#1777 = VERTEX_POINT ( 'NONE', #6063 ) ;
#1778 = EDGE_CURVE ( 'NONE', #8159, #3937, #2902, .T. ) ;
#1779 = CARTESIAN_POINT ( 'NONE',  ( 9.869213319667256457, -7.750000000000000000, 0.000000000000000000 ) ) ;
#1780 = FACE_OUTER_BOUND ( 'NONE', #1705, .T. ) ;
#1781 = ORIENTED_EDGE ( 'NONE', *, *, #6468, .T. ) ;
#1782 = CIRCLE ( 'NONE', #7705, 1.599999999999992983 ) ;
#1783 = CARTESIAN_POINT ( 'NONE',  ( 0.000000000000000000, -19.00000000000000711, -1.249999999999997558 ) ) ;
#1784 =( LENGTH_UNIT ( ) NAMED_UNIT ( * ) SI_UNIT ( .MILLI., .METRE. ) );
#1785 = VERTEX_POINT ( 'NONE', #8578 ) ;
#1786 = CARTESIAN_POINT ( 'NONE',  ( -4.089228379062038066, 4.089228379062021190, 2.099999999999999201 ) ) ;
#1787 = CARTESIAN_POINT ( 'NONE',  ( -4.173491630687863108, -2.231261971483782691, 5.336051716722022498 ) ) ;
#1788 = DIRECTION ( 'NONE',  ( -0.000000000000000000, 0.000000000000000000, 1.000000000000000000 ) ) ;
#1789 = ORIENTED_EDGE ( 'NONE', *, *, #7459, .F. ) ;
#1790 = CIRCLE ( 'NONE', #3138, 1.599999999999992983 ) ;
#1791 = EDGE_LOOP ( 'NONE', ( #4232, #4106, #4971, #10229 ) ) ;
#1792 = FACE_OUTER_BOUND ( 'NONE', #939, .T. ) ;
#1793 = DIRECTION ( 'NONE',  ( -1.000000000000000000, -1.156482317317871478E-16, 0.000000000000000000 ) ) ;
#1794 = EDGE_LOOP ( 'NONE', ( #779, #4050 ) ) ;
#1795 = CARTESIAN_POINT ( 'NONE',  ( -5.432285873273256627, -0.8603895577212797852, 4.479999999999999538 ) ) ;
#1796 = CARTESIAN_POINT ( 'NONE',  ( 2.496947748567516889, -4.900535883036019946, 0.8399999999999999689 ) ) ;
#1797 = CARTESIAN_POINT ( 'NONE',  ( -5.152728359536494551, -2.625446233515535077, 4.339999999999999858 ) ) ;
#1798 = ORIENTED_EDGE ( 'NONE', *, *, #4717, .F. ) ;
#1799 = AXIS2_PLACEMENT_3D ( 'NONE', #4449, #6195, #7698 ) ;
#1800 = CARTESIAN_POINT ( 'NONE',  ( 1.229367062500000163, -13.00000000000000533, -1.718750000682796486 ) ) ;
#1801 = AXIS2_PLACEMENT_3D ( 'NONE', #73, #2664, #1766 ) ;
#1802 = VERTEX_POINT ( 'NONE', #4484 ) ;
#1803 = DIRECTION ( 'NONE',  ( -5.694029147589358720E-15, -6.585044023479645679E-31, 1.000000000000000000 ) ) ;
#1804 = LINE ( 'NONE', #5030, #2388 ) ;
#1805 = CARTESIAN_POINT ( 'NONE',  ( -1.500000000000000222, -13.00000000000000533, -0.8125000013655935271 ) ) ;
#1806 = ORIENTED_EDGE ( 'NONE', *, *, #3812, .F. ) ;
#1807 = CARTESIAN_POINT ( 'NONE',  ( 1.272613240716556016, -10.02539999999999942, -12.00000000000000000 ) ) ;
#1808 = CARTESIAN_POINT ( 'NONE',  ( -1.229367062500000163, -12.29022459553277002, -1.135416667349463449 ) ) ;
#1809 = EDGE_CURVE ( 'NONE', #4861, #5471, #195, .T. ) ;
#1810 = CARTESIAN_POINT ( 'NONE',  ( -3.279728542977953687, 3.411736077305369541, 1.103948283277976561 ) ) ;
#1811 = ORIENTED_EDGE ( 'NONE', *, *, #9195, .F. ) ;
#1812 = DIRECTION ( 'NONE',  ( 0.000000000000000000, 0.000000000000000000, 1.000000000000000000 ) ) ;
#1813 = CARTESIAN_POINT ( 'NONE',  ( -2.625446233515515981, -5.152728359536500768, 1.259999999999999787 ) ) ;
#1814 = LINE ( 'NONE', #3454, #9036 ) ;
#1815 = EDGE_CURVE ( 'NONE', #9178, #9951, #3791, .T. ) ;
#1816 = CARTESIAN_POINT ( 'NONE',  ( 4.089228379062037178, -4.089228379062022967, 3.499999999999999112 ) ) ;
#1817 =( REPRESENTATION_RELATIONSHIP ('NONE','NONE', #5100, #7207 ) REPRESENTATION_RELATIONSHIP_WITH_TRANSFORMATION ( #7426 )SHAPE_REPRESENTATION_RELATIONSHIP( ) );
#1818 = CARTESIAN_POINT ( 'NONE',  ( 23.86937280323380506, 6.000000000000001776, -12.00000000000000000 ) ) ;
#1819 = DIRECTION ( 'NONE',  ( 0.3420201433256627732, 0.9396926207859105373, 0.000000000000000000 ) ) ;
#1820 = DIRECTION ( 'NONE',  ( 0.000000000000000000, -0.000000000000000000, -1.000000000000000000 ) ) ;
#1821 = CARTESIAN_POINT ( 'NONE',  ( 4.687928535947288644, -0.6479879772514620662, 1.416051716722023235 ) ) ;
#1822 = CARTESIAN_POINT ( 'NONE',  ( -1.229367062500000163, -12.29022459553277002, -2.010416667349463005 ) ) ;
#1823 = CARTESIAN_POINT ( 'NONE',  ( -3.279728542977953687, 3.411736077305369541, 3.903948283277975939 ) ) ;
#1824 = CARTESIAN_POINT ( 'NONE',  ( 8.692241771943170539E-17, -11.58044919106553650, -2.593750000682796486 ) ) ;
#1825 = ORIENTED_EDGE ( 'NONE', *, *, #4857, .F. ) ;
#1826 = ADVANCED_FACE ( 'NONE', ( #6972, #7023 ), #6870, .T. ) ;
#1827 = CARTESIAN_POINT ( 'NONE',  ( -3.826313983664925811, -3.951860609387098489, 5.196051716722022817 ) ) ;
#1828 = DIRECTION ( 'NONE',  ( -1.000000000000000000, -0.000000000000000000, -0.000000000000000000 ) ) ;
#1829 = DIRECTION ( 'NONE',  ( -1.000000000000000000, 0.000000000000000000, 0.000000000000000000 ) ) ;
#1830 = VERTEX_POINT ( 'NONE', #6122 ) ;
#1831 = PLANE ( 'NONE',  #5231 ) ;
#1832 = DIRECTION ( 'NONE',  ( -1.000000000000000000, 0.000000000000000000, 0.000000000000000000 ) ) ;
#1833 = ORIENTED_EDGE ( 'NONE', *, *, #6506, .T. ) ;
#1834 = CARTESIAN_POINT ( 'NONE',  ( -4.687928535947287756, 0.6479879772514611780, 11.21605171672202417 ) ) ;
#1835 = EDGE_CURVE ( 'NONE', #6218, #9020, #1774, .T. ) ;
#1836 =( BOUNDED_CURVE ( )  B_SPLINE_CURVE ( 2, ( #4860, #6497, #10451, #5603, #8105, #788, #4018 ),
 .UNSPECIFIED., .F., .T. ) 
 B_SPLINE_CURVE_WITH_KNOTS ( ( 3, 2, 2, 3 ),
 ( 0.3333333333333333148, 0.3611111111111111049, 0.3888888888888888395, 0.4166666666666666297 ),
 .UNSPECIFIED. ) 
 CURVE ( )  GEOMETRIC_REPRESENTATION_ITEM ( )  RATIONAL_B_SPLINE_CURVE ( ( 1.000000000000000000, 0.8660254037844387076, 1.000000000000000000, 0.8660254037844387076, 1.000000000000000000, 0.8660254037844389297, 0.9999999999999997780 ) ) 
 REPRESENTATION_ITEM ( '' )  );
#1837 = CARTESIAN_POINT ( 'NONE',  ( -1.229367062500000163, -12.29022459553277002, -2.635416667349463449 ) ) ;
#1838 = ADVANCED_FACE ( 'NONE', ( #6916 ), #3691, .T. ) ;
#1839 = ORIENTED_EDGE ( 'NONE', *, *, #3054, .F. ) ;
#1840 = CARTESIAN_POINT ( 'NONE',  ( -4.000000000000000888, 19.99999999999999645, 15.00000000000000000 ) ) ;
#1841 = ORIENTED_EDGE ( 'NONE', *, *, #4751, .F. ) ;
#1842 = CARTESIAN_POINT ( 'NONE',  ( 2.697157280332745266, -7.750000000000000000, 0.000000000000000000 ) ) ;
#1843 = DIRECTION ( 'NONE',  ( -0.000000000000000000, -0.000000000000000000, -1.000000000000000000 ) ) ;
#1844 = ORIENTED_EDGE ( 'NONE', *, *, #5107, .T. ) ;
#1845 = CARTESIAN_POINT ( 'NONE',  ( 2.496947748567516889, -4.900535883036019946, 12.03999999999999915 ) ) ;
#1846 = CARTESIAN_POINT ( 'NONE',  ( -2.496947748567517333, 4.900535883036019058, 7.839999999999999858 ) ) ;
#1847 = CARTESIAN_POINT ( 'NONE',  ( -5.711843387010018702, 0.9046671180729746187, 7.419999999999998153 ) ) ;
#1848 = ORIENTED_EDGE ( 'NONE', *, *, #5300, .T. ) ;
#1849 = CARTESIAN_POINT ( 'NONE',  ( -1.229367062500000163, -12.29022459553277002, -0.01041666734946308792 ) ) ;
#1850 = EDGE_CURVE ( 'NONE', #9178, #4330, #2161, .T. ) ;
#1851 = SHAPE_REPRESENTATION_RELATIONSHIP ( 'NONE' , 'NONE' ,  #8347, #689 ) ;
#1852 = VECTOR ( 'NONE', #886, 1000.000000000000000 ) ;
#1853 = ORIENTED_EDGE ( 'NONE', *, *, #7768, .F. ) ;
#1854 = CARTESIAN_POINT ( 'NONE',  ( 10.00000000000000000, -5.979767908488829775, -1.814490771706245065 ) ) ;
#1855 = AXIS2_PLACEMENT_3D ( 'NONE', #8574, #7021, #4689 ) ;
#1856 = DIRECTION ( 'NONE',  ( -0.9396926207859105373, 0.3420201433256627732, 0.000000000000000000 ) ) ;
#1857 = EDGE_LOOP ( 'NONE', ( #8302, #4110, #3466, #8986 ) ) ;
#1858 = CARTESIAN_POINT ( 'NONE',  ( 23.26376179071655770, -10.02539999999999942, 0.000000000000000000 ) ) ;
#1859 = AXIS2_PLACEMENT_3D ( 'NONE', #7384, #75, #2411 ) ;
#1860 = CARTESIAN_POINT ( 'NONE',  ( -1.229367062500000163, -13.70977540446723708, -2.552083334016129967 ) ) ;
#1861 = CARTESIAN_POINT ( 'NONE',  ( 1.963858260114715870, -4.049832306626327316, 2.643948283277976596 ) ) ;
#1862 = ORIENTED_EDGE ( 'NONE', *, *, #2628, .T. ) ;
#1863 = CARTESIAN_POINT ( 'NONE',  ( -17.00000000000000000, 19.99999999999999645, -9.000000000000000000 ) ) ;
#1864 = CIRCLE ( 'NONE', #3879, 6.248999999999999666 ) ;
#1865 = CARTESIAN_POINT ( 'NONE',  ( 0.8603895577212593571, 5.432285873273261068, 10.91999999999999993 ) ) ;
#1866 = CARTESIAN_POINT ( 'NONE',  ( -5.999999999999999112, 26.99999999999999289, -14.00000000000000178 ) ) ;
#1867 = CARTESIAN_POINT ( 'NONE',  ( -5.711843387010019590, 0.9046671180729746187, 4.620000000000000107 ) ) ;
#1868 = AXIS2_PLACEMENT_3D ( 'NONE', #5235, #2910, #6230 ) ;
#1869 = DIRECTION ( 'NONE',  ( 0.9396926207859105373, -0.3420201433256627732, 0.000000000000000000 ) ) ;
#1870 =( GEOMETRIC_REPRESENTATION_CONTEXT ( 3 ) GLOBAL_UNCERTAINTY_ASSIGNED_CONTEXT ( ( #3256 ) ) GLOBAL_UNIT_ASSIGNED_CONTEXT ( ( #8779, #8724, #8618 ) ) REPRESENTATION_CONTEXT ( 'NONE', 'WORKASPACE' ) );
#1871 = CARTESIAN_POINT ( 'NONE',  ( -1.499999999999999778, -12.13397459621556784, -1.854166668032260379 ) ) ;
#1872 = CARTESIAN_POINT ( 'NONE',  ( 10.00000000000000000, -5.349675154362301122, -3.229702268444983648 ) ) ;
#1873 = CARTESIAN_POINT ( 'NONE',  ( 2.122056237541221524, -3.969226411068978777, 4.636051716722022320 ) ) ;
#1874 = CARTESIAN_POINT ( 'NONE',  ( -2.607672531582950546E-16, -14.41955080893447416, -1.843750000682796708 ) ) ;
#1875 = CIRCLE ( 'NONE', #9672, 1.599999999999998979 ) ;
#1876 = CARTESIAN_POINT ( 'NONE',  ( -3.279728542977953687, 3.411736077305369541, 1.103948283277976561 ) ) ;
#1877 = FACE_BOUND ( 'NONE', #7579, .T. ) ;
#1879 = ORIENTED_EDGE ( 'NONE', *, *, #264, .T. ) ;
#1878 = VECTOR ( 'NONE', #6081, 1000.000000000000000 ) ;
#1880 = CARTESIAN_POINT ( 'NONE',  ( 5.110351332421769754, 2.708615832122969191, 6.736051716722023741 ) ) ;
#1881 = AXIS2_PLACEMENT_3D ( 'NONE', #8069, #8855, #3978 ) ;
#1882 = DIRECTION ( 'NONE',  ( 0.000000000000000000, 0.000000000000000000, 1.000000000000000000 ) ) ;
#1883 = CIRCLE ( 'NONE', #8988, 8.500000000000000000 ) ;
#1884 = DIRECTION ( 'NONE',  ( 1.000000000000000000, -0.000000000000000000, -0.000000000000000000 ) ) ;
#1885 = ORIENTED_EDGE ( 'NONE', *, *, #6222, .T. ) ;
#1886 = ADVANCED_FACE ( 'NONE', ( #7778 ), #6175, .F. ) ;
#1887 = DIRECTION ( 'NONE',  ( -0.000000000000000000, -0.000000000000000000, 1.000000000000000000 ) ) ;
#1888 = AXIS2_PLACEMENT_3D ( 'NONE', #509, #8621, #9480 ) ;
#1889 = CARTESIAN_POINT ( 'NONE',  ( -0.8323763977770610722, 4.658724279160015413, 8.976051716722020402 ) ) ;
#1890 = VECTOR ( 'NONE', #1828, 1000.000000000000000 ) ;
#1891 = DIRECTION ( 'NONE',  ( 1.000000000000000000, 0.000000000000000000, 0.000000000000000000 ) ) ;
#1892 = ORIENTED_EDGE ( 'NONE', *, *, #6016, .T. ) ;
#1893 = CARTESIAN_POINT ( 'NONE',  ( 0.000000000000000000, 0.000000000000000000, 30.00000000000000711 ) ) ;
#1894 = VERTEX_POINT ( 'NONE', #5381 ) ;
#1895 = DIRECTION ( 'NONE',  ( -1.000000000000000000, -0.000000000000000000, -0.000000000000000000 ) ) ;
#1896 = ADVANCED_FACE ( 'NONE', ( #2846 ), #1357, .F. ) ;
#1897 = PLANE ( 'NONE',  #8642 ) ;
#1898 = ORIENTED_EDGE ( 'NONE', *, *, #3463, .F. ) ;
#1899 = EDGE_CURVE ( 'NONE', #8785, #9003, #3936, .T. ) ;
#1900 = CARTESIAN_POINT ( 'NONE',  ( 5.726445515403654873, -0.8124729078101852187, 4.216051716722023279 ) ) ;
#1901 = EDGE_CURVE ( 'NONE', #7181, #798, #2211, .T. ) ;
#1902 = CARTESIAN_POINT ( 'NONE',  ( 5.152728359536493663, 2.625446233515533745, 5.739999999999997549 ) ) ;
#1903 = CARTESIAN_POINT ( 'NONE',  ( -5.432285873273256627, -0.8603895577212797852, 7.279999999999999361 ) ) ;
#1904 = ORIENTED_EDGE ( 'NONE', *, *, #9554, .F. ) ;
#1905 = CARTESIAN_POINT ( 'NONE',  ( 1.229367062500000163, -13.00000000000000533, -0.7187500006827964860 ) ) ;
#1906 =( LENGTH_UNIT ( ) NAMED_UNIT ( * ) SI_UNIT ( .MILLI., .METRE. ) );
#1907 = ORIENTED_EDGE ( 'NONE', *, *, #4497, .F. ) ;
#1908 = LINE ( 'NONE', #3336, #9063 ) ;
#1909 = PLANE ( 'NONE',  #503 ) ;
#1910 = ORIENTED_EDGE ( 'NONE', *, *, #1388, .F. ) ;
#1911 = ADVANCED_FACE ( 'NONE', ( #5437 ), #5333, .T. ) ;
#1912 = DIRECTION ( 'NONE',  ( -1.000000000000000000, -0.000000000000000000, -0.000000000000000000 ) ) ;
#1913 = DIRECTION ( 'NONE',  ( -0.9396926207859105373, -0.3420201433256627732, 0.000000000000000000 ) ) ;
#1914 = CARTESIAN_POINT ( 'NONE',  ( 1.229367062500000163, -13.00000000000000533, -2.343750000682796486 ) ) ;
#1915 = CARTESIAN_POINT ( 'NONE',  ( -4.658724279160018078, 0.8323763977770419764, 6.423948283277978177 ) ) ;
#1916 = EDGE_LOOP ( 'NONE', ( #10342, #10284, #8668 ) ) ;
#1917 = CARTESIAN_POINT ( 'NONE',  ( 13.83898384071655840, 6.025400000000000311, 0.000000000000000000 ) ) ;
#1918 = CARTESIAN_POINT ( 'NONE',  ( 5.432285873273257515, 0.8603895577212793411, 11.47999999999999865 ) ) ;
#1919 = DIRECTION ( 'NONE',  ( -1.000000000000000000, -0.000000000000000000, -0.000000000000000000 ) ) ;
#1920 = CARTESIAN_POINT ( 'NONE',  ( 2.625446233515515093, 5.152728359536503433, 5.459999999999999076 ) ) ;
#1921 = AXIS2_PLACEMENT_3D ( 'NONE', #4104, #7391, #9842 ) ;
#1922 = DIRECTION ( 'NONE',  ( 0.000000000000000000, 0.000000000000000000, 1.000000000000000000 ) ) ;
#1923 = PLANE ( 'NONE',  #6861 ) ;
#1924 = CARTESIAN_POINT ( 'NONE',  ( -2.000000000000000000, 1.693568526656785686E-17, 2.343061888689530026 ) ) ;
#1925 = CARTESIAN_POINT ( 'NONE',  ( 4.687928535947288644, -0.6479879772514620662, 12.61605171672202097 ) ) ;
#1926 = FACE_OUTER_BOUND ( 'NONE', #3493, .T. ) ;
#1927 = PRODUCT_RELATED_PRODUCT_CATEGORY ( 'part', '', ( #4517 ) ) ;
#1928 = CARTESIAN_POINT ( 'NONE',  ( 4.023224611898322145, -4.155232146225737111, -0.2960517167220233503 ) ) ;
#1929 = AXIS2_PLACEMENT_3D ( 'NONE', #5827, #7325, #3245 ) ;
#1930 = CARTESIAN_POINT ( 'NONE',  ( -1.229367062500000163, -12.29022459553277002, -0.5104166673494631157 ) ) ;
#1931 = ORIENTED_EDGE ( 'NONE', *, *, #7531, .T. ) ;
#1932 = CARTESIAN_POINT ( 'NONE',  ( 2.542276634908080535, 5.195105386651229118, 6.456051716722022604 ) ) ;
#1933 = DIRECTION ( 'NONE',  ( 0.3420201433256627732, 0.9396926207859105373, -0.000000000000000000 ) ) ;
#1934 = CARTESIAN_POINT ( 'NONE',  ( -26.99999999999998934, 34.99999999999999289, 5.999999999999999112 ) ) ;
#1935 = EDGE_LOOP ( 'NONE', ( #2857, #2703, #8254, #2112 ) ) ;
#1936 = CIRCLE ( 'NONE', #3614, 2.000000000000000000 ) ;
#1937 = CARTESIAN_POINT ( 'NONE',  ( 2.042957248827968808, -4.009529358847652603, 12.03999999999999915 ) ) ;
#1938 = SURFACE_SIDE_STYLE ('',( #5055 ) ) ;
#1939 = CARTESIAN_POINT ( 'NONE',  ( -2.148092372876330813, -4.215868657802593233, 1.259999999999999787 ) ) ;
#1940 = DIRECTION ( 'NONE',  ( 1.049727191138616477E-16, 0.5150380749100571531, -0.8571673007021105573 ) ) ;
#1941 = EDGE_LOOP ( 'NONE', ( #4951, #8464, #501, #6269, #6928, #7301, #2227, #4780, #1496, #7452, #395, #571, #9854, #4785, #4974, #3444, #1841, #9369, #3896, #2750, #9597, #5523, #991, #5584, #1688, #4478, #8851, #9373, #1853, #983, #3480, #7131, #3072, #3749, #10331, #5812, #1153, #8634, #4260, #1798, #4184, #8716, #6045, #8263, #10050, #10397 ) ) ;
#1942 = CARTESIAN_POINT ( 'NONE',  ( 3.999999999999999112, 20.00000000000000000, -15.00000000000000000 ) ) ;
#1943 = EDGE_CURVE ( 'NONE', #65, #8703, #7302, .T. ) ;
#1944 = VERTEX_POINT ( 'NONE', #8781 ) ;
#1945 = DIRECTION ( 'NONE',  ( 0.000000000000000000, 1.000000000000000000, -0.000000000000000000 ) ) ;
#1946 = VECTOR ( 'NONE', #7415, 1000.000000000000000 ) ;
#1947 = DIRECTION ( 'NONE',  ( 0.000000000000000000, 0.000000000000000000, -1.000000000000000000 ) ) ;
#1948 = ORIENTED_EDGE ( 'NONE', *, *, #6566, .T. ) ;
#1949 = CARTESIAN_POINT ( 'NONE',  ( 0.9046671180729951578, -5.711843387010016926, 12.17999999999999439 ) ) ;
#1950 = CARTESIAN_POINT ( 'NONE',  ( -3.889087296526005044, -3.889087296526019255, 1.399999999999999689 ) ) ;
#1951 = CARTESIAN_POINT ( 'NONE',  ( 13.83898384071655840, 6.025400000000000311, -12.00000000000000000 ) ) ;
#1952 = CARTESIAN_POINT ( 'NONE',  ( 4.089228379062037178, -4.089228379062022967, 9.099999999999999645 ) ) ;
#1953 = ORIENTED_EDGE ( 'NONE', *, *, #3125, .T. ) ;
#1954 = CARTESIAN_POINT ( 'NONE',  ( -1.229367062500000163, -13.00000000000000533, -0.9687500006827964860 ) ) ;
#1955 = VECTOR ( 'NONE', #4995, 1000.000000000000000 ) ;
#1956 = EDGE_CURVE ( 'NONE', #7946, #8610, #7812, .T. ) ;
#1957 = EDGE_CURVE ( 'NONE', #4491, #10281, #7132, .T. ) ;
#1958 = VERTEX_POINT ( 'NONE', #3060 ) ;
#1959 = CARTESIAN_POINT ( 'NONE',  ( 1.300000000000000044, 1.108512516844082141, 0.6399999999999991251 ) ) ;
#1960 = CARTESIAN_POINT ( 'NONE',  ( 10.68814634676619590, -10.00000000000000000, 0.000000000000000000 ) ) ;
#1961 = ORIENTED_EDGE ( 'NONE', *, *, #2220, .T. ) ;
#1962 = CARTESIAN_POINT ( 'NONE',  ( 0.000000000000000000, 6.000000000000000000, 0.000000000000000000 ) ) ;
#1963 = VECTOR ( 'NONE', #2407, 1000.000000000000000 ) ;
#1964 = DIRECTION ( 'NONE',  ( -1.000000000000000000, 0.000000000000000000, 0.000000000000000000 ) ) ;
#1965 = CARTESIAN_POINT ( 'NONE',  ( -1.229367062500000163, -13.00000000000000533, -0.09375000068279679133 ) ) ;
#1966 = CARTESIAN_POINT ( 'NONE',  ( 5.195105386651219348, 2.542276634908100075, -0.8560517167220232926 ) ) ;
#1967 = EDGE_LOOP ( 'NONE', ( #7031, #8687, #5104, #4482 ) ) ;
#1968 = AXIS2_PLACEMENT_3D ( 'NONE', #4462, #8603, #7710 ) ;
#1969 = PLANE ( 'NONE',  #8818 ) ;
#1970 = DIRECTION ( 'NONE',  ( 0.3420201433256627732, 0.9396926207859105373, 0.000000000000000000 ) ) ;
#1971 = EDGE_CURVE ( 'NONE', #5116, #1459, #3575, .T. ) ;
#1972 = CARTESIAN_POINT ( 'NONE',  ( -0.7499999999999997780, -11.70096189432334555, 0.1041666653010730748 ) ) ;
#1973 = CIRCLE ( 'NONE', #6013, 2.000000000000000000 ) ;
#1974 = CARTESIAN_POINT ( 'NONE',  ( 1.500000000000000222, -13.00000000000000533, 0.000000000000000000 ) ) ;
#1975 = VECTOR ( 'NONE', #7045, 1000.000000000000000 ) ;
#1976 = CARTESIAN_POINT ( 'NONE',  ( 7.546553696766195252, -10.00000000000000000, 0.000000000000000000 ) ) ;
#1977 = CARTESIAN_POINT ( 'NONE',  ( -2.000000000000000000, -7.063614741696270016, 0.000000000000000000 ) ) ;
#1978 = LINE ( 'NONE', #970, #3384 ) ;
#1979 = CARTESIAN_POINT ( 'NONE',  ( 3.411736077305382420, -3.279728542977940364, 10.09605171672202140 ) ) ;
#1980 = CARTESIAN_POINT ( 'NONE',  ( -1.229367062500000163, -12.29022459553277002, -1.010416667349463449 ) ) ;
#1981 = CARTESIAN_POINT ( 'NONE',  ( -0.6479879772514802738, 4.687928535947285091, 9.783948283277975833 ) ) ;
#1982 = EDGE_CURVE ( 'NONE', #1996, #6164, #9642, .T. ) ;
#1983 = CARTESIAN_POINT ( 'NONE',  ( -2.607672531582950546E-16, -14.41955080893447416, -1.343750000682796486 ) ) ;
#1984 = VERTEX_POINT ( 'NONE', #3956 ) ;
#1985 = CARTESIAN_POINT ( 'NONE',  ( 0.7727076532861471003, 5.446173322633805824, 9.116051716722020970 ) ) ;
#1986 = CARTESIAN_POINT ( 'NONE',  ( 21.54671318033274829, -7.750000000000000000, 0.000000000000000000 ) ) ;
#1987 = DIRECTION ( 'NONE',  ( 0.000000000000000000, -8.673617379884032514E-16, -1.000000000000000000 ) ) ;
#1988 = ORIENTED_EDGE ( 'NONE', *, *, #1379, .F. ) ;
#1989 = CARTESIAN_POINT ( 'NONE',  ( -3.345732310141667831, 3.345732310141653620, 7.699999999999998401 ) ) ;
#1990 = DIRECTION ( 'NONE',  ( -0.000000000000000000, -1.000000000000000000, -0.000000000000000000 ) ) ;
#1991 = EDGE_CURVE ( 'NONE', #1478, #8065, #1468, .T. ) ;
#1992 = CARTESIAN_POINT ( 'NONE',  ( 3.119207202478379681, 3.244753828200549695, 14.99605171672202175 ) ) ;
#1993 = CARTESIAN_POINT ( 'NONE',  ( -1.229367062500000385, -13.70977540446723886, -2.052083334016129967 ) ) ;
#1994 = EDGE_LOOP ( 'NONE', ( #3224, #6584, #2790, #9112 ) ) ;
#1995 = DIRECTION ( 'NONE',  ( 0.000000000000000000, 0.000000000000000000, 1.000000000000000000 ) ) ;
#1996 = VERTEX_POINT ( 'NONE', #8839 ) ;
#1997 = EDGE_CURVE ( 'NONE', #9192, #7510, #9589, .T. ) ;
#1998 = DIRECTION ( 'NONE',  ( 1.000000000000000000, 0.000000000000000000, 0.000000000000000000 ) ) ;
#1999 = CARTESIAN_POINT ( 'NONE',  ( -2.499999999999992895, -28.99999999999999289, 3.061616997868383141E-16 ) ) ;
#2000 = DIRECTION ( 'NONE',  ( 0.3420201433256627732, -0.9396926207859105373, 0.000000000000000000 ) ) ;
#2001 = VERTEX_POINT ( 'NONE', #5594 ) ;
#2002 = CARTESIAN_POINT ( 'NONE',  ( -0.9046671180729963790, 5.711843387010016926, 10.77999999999999936 ) ) ;
#2003 = CARTESIAN_POINT ( 'NONE',  ( 5.432285873273257515, 0.8603895577212793411, 8.679999999999997939 ) ) ;
#2004 = CARTESIAN_POINT ( 'NONE',  ( 2.496947748567516889, -4.900535883036019946, 6.439999999999999503 ) ) ;
#2005 = VERTEX_POINT ( 'NONE', #6387 ) ;
#2006 = CARTESIAN_POINT ( 'NONE',  ( -0.7499999999999997780, -11.70096189432334555, -1.333333333333333481 ) ) ;
#2007 = EDGE_CURVE ( 'NONE', #8580, #2344, #9689, .T. ) ;
#2008 = ORIENTED_EDGE ( 'NONE', *, *, #7002, .T. ) ;
#2009 = CARTESIAN_POINT ( 'NONE',  ( 1.500000000000000222, -13.00000000000000533, -2.500000000000000000 ) ) ;
#2010 = FACE_OUTER_BOUND ( 'NONE', #5588, .T. ) ;
#2011 = ORIENTED_EDGE ( 'NONE', *, *, #8140, .T. ) ;
#2012 = DIRECTION ( 'NONE',  ( 0.000000000000000000, 0.000000000000000000, -1.000000000000000000 ) ) ;
#2013 = CARTESIAN_POINT ( 'NONE',  ( 1.300000000000000044, 0.7390083445627193548, -1.280000000000000693 ) ) ;
#2014 = CARTESIAN_POINT ( 'NONE',  ( 5.010572059283444624, -10.02539999999999942, -12.00000000000000000 ) ) ;
#2015 = CARTESIAN_POINT ( 'NONE',  ( 1.963858260114715870, -4.049832306626327316, 8.243948283277976685 ) ) ;
#2016 = ORIENTED_EDGE ( 'NONE', *, *, #21, .T. ) ;
#2017 = DIRECTION ( 'NONE',  ( 0.000000000000000000, -4.263256414560601746E-14, -1.000000000000000000 ) ) ;
#2018 = VECTOR ( 'NONE', #1408, 1000.000000000000000 ) ;
#2019 = CARTESIAN_POINT ( 'NONE',  ( -4.900535883036028828, 2.496947748567499126, 13.15999999999999837 ) ) ;
#2020 = DIRECTION ( 'NONE',  ( 0.000000000000000000, 0.000000000000000000, 1.000000000000000000 ) ) ;
#2021 = CARTESIAN_POINT ( 'NONE',  ( -2.625446233515515537, -5.152728359536502545, 12.45999999999999730 ) ) ;
#2022 = CARTESIAN_POINT ( 'NONE',  ( -15.00000000000000000, 19.99999999999999645, -9.000000000000000000 ) ) ;
#2023 = CARTESIAN_POINT ( 'NONE',  ( -31.74999999999995737, 0.000000000000000000, 0.000000000000000000 ) ) ;
#2024 = VECTOR ( 'NONE', #550, 1000.000000000000000 ) ;
#2025 = DIRECTION ( 'NONE',  ( 0.000000000000000000, 0.000000000000000000, 1.000000000000000000 ) ) ;
#2026 = CARTESIAN_POINT ( 'NONE',  ( -3.411736077305382420, 3.279728542977939476, 8.696051716722022817 ) ) ;
#2027 = EDGE_CURVE ( 'NONE', #4853, #7886, #6784, .T. ) ;
#2028 = AXIS2_PLACEMENT_3D ( 'NONE', #2953, #1466, #1305 ) ;
#2029 = EDGE_CURVE ( 'NONE', #4487, #3187, #5487, .T. ) ;
#2030 = CARTESIAN_POINT ( 'NONE',  ( -1.229367062500000385, -13.70977540446723886, -1.927083334016129745 ) ) ;
#2031 = CARTESIAN_POINT ( 'NONE',  ( -2.231261971483764484, -4.173491630687871101, 11.46394828327797555 ) ) ;
#2032 = CARTESIAN_POINT ( 'NONE',  ( -1.229367062500000163, -13.00000000000000533, -0.9687500006827964860 ) ) ;
#2033 = AXIS2_PLACEMENT_3D ( 'NONE', #10337, #9649, #2376 ) ;
#2034 = VERTEX_POINT ( 'NONE', #3109 ) ;
#2035 = DIRECTION ( 'NONE',  ( 0.000000000000000000, 0.000000000000000000, 1.000000000000000000 ) ) ;
#2036 = DIRECTION ( 'NONE',  ( 1.000000000000000000, 0.000000000000000000, 0.000000000000000000 ) ) ;
#2037 = CARTESIAN_POINT ( 'NONE',  ( 0.000000000000000000, 6.000000000000000000, -12.00000000000000000 ) ) ;
#2038 = ORIENTED_EDGE ( 'NONE', *, *, #3451, .T. ) ;
#2039 = EDGE_CURVE ( 'NONE', #10462, #144, #1334, .T. ) ;
#2040 = STYLED_ITEM ( 'NONE', ( #5855 ), #7952 ) ;
#2041 = CARTESIAN_POINT ( 'NONE',  ( -4.673326407553653361, 0.7401821875142517992, 7.419999999999999041 ) ) ;
#2042 = SURFACE_SIDE_STYLE ('',( #6743 ) ) ;
#2043 = AXIS2_PLACEMENT_3D ( 'NONE', #5399, #4503, #8643 ) ;
#2044 = CARTESIAN_POINT ( 'NONE',  ( 0.7401821875142697849, -4.673326407553650697, 0.9799999999999997602 ) ) ;
#2045 = CARTESIAN_POINT ( 'NONE',  ( 8.692241771943169307E-17, -11.58044919106553294, -0.2187500006827968746 ) ) ;
#2046 = VERTEX_POINT ( 'NONE', #3670 ) ;
#2047 = AXIS2_PLACEMENT_3D ( 'NONE', #4230, #7668, #6862 ) ;
#2048 = VECTOR ( 'NONE', #3939, 1000.000000000000000 ) ;
#2049 = EDGE_LOOP ( 'NONE', ( #4459, #1298, #8039, #4474 ) ) ;
#2050 = PLANE ( 'NONE',  #6514 ) ;
#2051 = DIRECTION ( 'NONE',  ( 0.000000000000000000, 0.000000000000000000, 1.000000000000000000 ) ) ;
#2052 = VECTOR ( 'NONE', #8348, 1000.000000000000000 ) ;
#2053 = DIRECTION ( 'NONE',  ( 0.000000000000000000, -0.000000000000000000, 1.000000000000000000 ) ) ;
#2054 = ORIENTED_EDGE ( 'NONE', *, *, #3622, .F. ) ;
#2055 = CARTESIAN_POINT ( 'NONE',  ( -0.7727076532861475444, -5.446173322633804048, 4.916051716722023457 ) ) ;
#2056 = CARTESIAN_POINT ( 'NONE',  ( -5.152728359536494551, -2.625446233515535077, 9.939999999999994174 ) ) ;
#2057 = VECTOR ( 'NONE', #4305, 1000.000000000000000 ) ;
#2058 = CARTESIAN_POINT ( 'NONE',  ( -5.432285873273256627, -0.8603895577212797852, 10.07999999999999829 ) ) ;
#2059 = ORIENTED_EDGE ( 'NONE', *, *, #712, .F. ) ;
#2060 = DIRECTION ( 'NONE',  ( -0.9396926207859105373, -0.3420201433256627732, 0.000000000000000000 ) ) ;
#2061 = UNCERTAINTY_MEASURE_WITH_UNIT (LENGTH_MEASURE( 1.000000000000000082E-05 ), #1397, 'distance_accuracy_value', 'NONE');
#2062 = FILL_AREA_STYLE ('',( #9321 ) ) ;
#2063 = ORIENTED_EDGE ( 'NONE', *, *, #9661, .F. ) ;
#2064 = DIRECTION ( 'NONE',  ( 0.000000000000000000, 0.000000000000000000, 1.000000000000000000 ) ) ;
#2065 = CYLINDRICAL_SURFACE ( 'NONE', #7098, 1.500000000000000222 ) ;
#2066 = ORIENTED_EDGE ( 'NONE', *, *, #10380, .T. ) ;
#2067 = DIRECTION ( 'NONE',  ( 0.000000000000000000, 0.000000000000000000, 1.000000000000000000 ) ) ;
#2068 = CARTESIAN_POINT ( 'NONE',  ( -2.000000000000000000, -6.200809695932781196, 0.7745709230444935978 ) ) ;
#2069 = FACE_OUTER_BOUND ( 'NONE', #262, .T. ) ;
#2070 = CARTESIAN_POINT ( 'NONE',  ( -3.969226411068985882, 2.122056237541205537, 6.563948283277975193 ) ) ;
#2071 = EDGE_LOOP ( 'NONE', ( #220, #10334, #2999, #7018 ) ) ;
#2072 = CARTESIAN_POINT ( 'NONE',  ( 0.7499999999999991118, -14.29903810567666333, -2.145833334698926897 ) ) ;
#2073 = CARTESIAN_POINT ( 'NONE',  ( -5.152728359536494551, -2.625446233515535077, 12.73999999999999488 ) ) ;
#2074 = CARTESIAN_POINT ( 'NONE',  ( 1.499999999999999778, -13.86602540378444637, 0.3958333319677397322 ) ) ;
#2075 = CARTESIAN_POINT ( 'NONE',  ( 0.9046671180729953798, -5.711843387010016926, 12.17999999999999616 ) ) ;
#2076 = EDGE_CURVE ( 'NONE', #8065, #2419, #6898, .T. ) ;
#2077 = DIRECTION ( 'NONE',  ( -0.000000000000000000, 1.000000000000000000, 0.000000000000000000 ) ) ;
#2078 = CARTESIAN_POINT ( 'NONE',  ( 17.58618750323380908, -10.00000000000000000, 0.000000000000000000 ) ) ;
#2079 = DIRECTION ( 'NONE',  ( -1.000000000000000000, -0.000000000000000000, -0.000000000000000000 ) ) ;
#2080 = CARTESIAN_POINT ( 'NONE',  ( 3.345732310141667387, -3.345732310141653620, 0.6999999999999997335 ) ) ;
#2081 = CARTESIAN_POINT ( 'NONE',  ( -1.229367062500000163, -12.29022459553277002, -0.5104166673494631157 ) ) ;
#2082 = CARTESIAN_POINT ( 'NONE',  ( -0.8124729078102072011, 5.726445515403652209, 4.183948283277976188 ) ) ;
#2083 = CARTESIAN_POINT ( 'NONE',  ( -1.229367062500000163, -13.00000000000000533, 0.03124999931720332663 ) ) ;
#2084 = ORIENTED_EDGE ( 'NONE', *, *, #2149, .T. ) ;
#2085 = AXIS2_PLACEMENT_3D ( 'NONE', #4386, #7632, #2808 ) ;
#2086 = ADVANCED_FACE ( 'NONE', ( #8556 ), #2142, .T. ) ;
#2087 = DIRECTION ( 'NONE',  ( 0.000000000000000000, 0.000000000000000000, 1.000000000000000000 ) ) ;
#2088 = EDGE_CURVE ( 'NONE', #6626, #9328, #2190, .T. ) ;
#2089 = DIRECTION ( 'NONE',  ( -1.000000000000000000, -0.000000000000000000, -0.000000000000000000 ) ) ;
#2090 = DIRECTION ( 'NONE',  ( 0.000000000000000000, 0.000000000000000000, -1.000000000000000000 ) ) ;
#2091 = CARTESIAN_POINT ( 'NONE',  ( 1.500000000000000222, -13.00000000000000533, -3.000000000000000000 ) ) ;
#2092 = ORIENTED_EDGE ( 'NONE', *, *, #8374, .F. ) ;
#2093 = CARTESIAN_POINT ( 'NONE',  ( -2.042957248827969252, 4.009529358847651714, 7.839999999999999858 ) ) ;
#2094 = VECTOR ( 'NONE', #2230, 1000.000000000000000 ) ;
#2095 = DIRECTION ( 'NONE',  ( 0.000000000000000000, 0.4999999999999992228, -0.8660254037844390407 ) ) ;
#2096 = CARTESIAN_POINT ( 'NONE',  ( -3.181980515339458027, -3.181980515339470905, 4.200000000000000178 ) ) ;
#2097 = CARTESIAN_POINT ( 'NONE',  ( -0.7500000000000007772, -14.29903810567666156, -2.666666666666666519 ) ) ;
#2098 = VERTEX_POINT ( 'NONE', #647 ) ;
#2099 = ADVANCED_FACE ( 'NONE', ( #6042 ), #6258, .F. ) ;
#2100 = ORIENTED_EDGE ( 'NONE', *, *, #6786, .T. ) ;
#2101 = AXIS2_PLACEMENT_3D ( 'NONE', #7090, #5610, #4547 ) ;
#2102 = DIRECTION ( 'NONE',  ( 0.000000000000000000, 0.000000000000000000, 1.000000000000000000 ) ) ;
#2103 = LINE ( 'NONE', #3584, #5082 ) ;
#2104 = ORIENTED_EDGE ( 'NONE', *, *, #2718, .F. ) ;
#2105 = CARTESIAN_POINT ( 'NONE',  ( -5.110351332421769754, -2.708615832122969191, 5.336051716722022498 ) ) ;
#2106 = CARTESIAN_POINT ( 'NONE',  ( 0.000000000000000000, 6.000000000000000000, -12.00000000000000000 ) ) ;
#2107 = ORIENTED_EDGE ( 'NONE', *, *, #2498, .F. ) ;
#2108 = DIRECTION ( 'NONE',  ( 0.000000000000000000, -0.5000000000000013323, -0.8660254037844378194 ) ) ;
#2109 = VECTOR ( 'NONE', #3652, 1000.000000000000000 ) ;
#2110 = ORIENTED_EDGE ( 'NONE', *, *, #3555, .T. ) ;
#2111 =( NAMED_UNIT ( * ) PLANE_ANGLE_UNIT ( ) SI_UNIT ( $, .RADIAN. ) );
#2112 = ORIENTED_EDGE ( 'NONE', *, *, #1436, .T. ) ;
#2113 = PLANE ( 'NONE',  #6176 ) ;
#2114 = STYLED_ITEM ( 'NONE', ( #8328 ), #2591 ) ;
#2115 = DIRECTION ( 'NONE',  ( 1.000000000000000000, -0.000000000000000000, -0.000000000000000000 ) ) ;
#2116 = ORIENTED_EDGE ( 'NONE', *, *, #8726, .T. ) ;
#2117 = DIRECTION ( 'NONE',  ( -1.000000000000000000, 0.000000000000000000, 0.000000000000000000 ) ) ;
#2118 = DIRECTION ( 'NONE',  ( 0.000000000000000000, -0.5000000000000009992, -0.8660254037844380415 ) ) ;
#2119 = CARTESIAN_POINT ( 'NONE',  ( -0.6479879772514802738, 4.687928535947285091, 6.983948283277976010 ) ) ;
#2120 = ORIENTED_EDGE ( 'NONE', *, *, #9280, .F. ) ;
#2121 = VECTOR ( 'NONE', #9568, 1000.000000000000000 ) ;
#2122 = DIRECTION ( 'NONE',  ( 0.000000000000000000, 0.000000000000000000, 1.000000000000000000 ) ) ;
#2123 = CARTESIAN_POINT ( 'NONE',  ( 1.658513752677435171, 6.603649639095712232, 0.000000000000000000 ) ) ;
#2124 = DIRECTION ( 'NONE',  ( 0.000000000000000000, 0.000000000000000000, -1.000000000000000000 ) ) ;
#2125 = CARTESIAN_POINT ( 'NONE',  ( 8.000000000000001776, 0.000000000000000000, 0.000000000000000000 ) ) ;
#2126 = VECTOR ( 'NONE', #3583, 1000.000000000000000 ) ;
#2127 = CARTESIAN_POINT ( 'NONE',  ( 1.500000000000000222, -12.13397459621556784, -2.458333333333333037 ) ) ;
#2128 = CARTESIAN_POINT ( 'NONE',  ( 22.43558391966725907, 3.750000000000000000, -12.00000000000000000 ) ) ;
#2129 = EDGE_CURVE ( 'NONE', #1478, #1396, #2246, .T. ) ;
#2130 = CARTESIAN_POINT ( 'NONE',  ( -2.000000000000015099, 35.00000000000000000, 3.999999999999986233 ) ) ;
#2131 = CIRCLE ( 'NONE', #5510, 0.1000000000000000472 ) ;
#2132 = CARTESIAN_POINT ( 'NONE',  ( -1.500000000000000222, -13.00000000000000533, -3.000000000000000000 ) ) ;
#2133 = CARTESIAN_POINT ( 'NONE',  ( 4.430710083317573655, 0.7916369971161595354, 9.676051716722021467 ) ) ;
#2134 = CARTESIAN_POINT ( 'NONE',  ( -1.229367062500000385, -13.70977540446723886, -1.552083334016130189 ) ) ;
#2135 = VECTOR ( 'NONE', #1250, 1000.000000000000000 ) ;
#2136 = EDGE_CURVE ( 'NONE', #6924, #1347, #8602, .T. ) ;
#2137 = CARTESIAN_POINT ( 'NONE',  ( 4.258245684917310037, 2.064922774268912686, 10.34394828327797633 ) ) ;
#2138 = CARTESIAN_POINT ( 'NONE',  ( 1.229367062500000163, -12.29022459553277002, -0.1770833340161300506 ) ) ;
#2139 = VECTOR ( 'NONE', #60, 1000.000000000000000 ) ;
#2140 = ORIENTED_EDGE ( 'NONE', *, *, #4588, .T. ) ;
#2141 = LINE ( 'NONE', #7653, #6437 ) ;
#2142 = CYLINDRICAL_SURFACE ( 'NONE', #5601, 8.500000000000000000 ) ;
#2143 = DIRECTION ( 'NONE',  ( -1.000000000000000000, -0.000000000000000000, -0.000000000000000000 ) ) ;
#2144 = CARTESIAN_POINT ( 'NONE',  ( 17.00000000000000000, 19.99999999999999645, -5.999999999999999112 ) ) ;
#2145 = ORIENTED_EDGE ( 'NONE', *, *, #2586, .F. ) ;
#2146 = CYLINDRICAL_SURFACE ( 'NONE', #6744, 3.000000000000000000 ) ;
#2147 = CARTESIAN_POINT ( 'NONE',  ( 12.12193523033274545, -7.750000000000000000, -12.00000000000000000 ) ) ;
#2148 = CARTESIAN_POINT ( 'NONE',  ( -2.148092372876330813, -4.215868657802593233, 4.059999999999999609 ) ) ;
#2149 = EDGE_CURVE ( 'NONE', #9328, #5890, #6155, .T. ) ;
#2150 = CARTESIAN_POINT ( 'NONE',  ( 1.229367062499999719, -13.70977540446724063, -0.3854166673494633932 ) ) ;
#2151 = ORIENTED_EDGE ( 'NONE', *, *, #8374, .T. ) ;
#2152 = ORIENTED_EDGE ( 'NONE', *, *, #1646, .F. ) ;
#2153 = DIRECTION ( 'NONE',  ( -0.9396926207859105373, -0.3420201433256627732, 0.000000000000000000 ) ) ;
#2154 = DIRECTION ( 'NONE',  ( 0.000000000000000000, 0.000000000000000000, 1.000000000000000000 ) ) ;
#2155 = ORIENTED_EDGE ( 'NONE', *, *, #9628, .T. ) ;
#2156 = CARTESIAN_POINT ( 'NONE',  ( -2.576046737280769605, 4.860232935257343456, 6.036051716722022675 ) ) ;
#2157 = SURFACE_SIDE_STYLE ('',( #5485 ) ) ;
#2158 = ORIENTED_EDGE ( 'NONE', *, *, #2029, .F. ) ;
#2159 = EDGE_CURVE ( 'NONE', #8622, #7022, #10153, .T. ) ;
#2160 = EDGE_CURVE ( 'NONE', #2545, #3971, #6104, .T. ) ;
#2161 = LINE ( 'NONE', #10124, #528 ) ;
#2162 = VERTEX_POINT ( 'NONE', #3037 ) ;
#2163 = ORIENTED_EDGE ( 'NONE', *, *, #6363, .F. ) ;
#2164 = DIRECTION ( 'NONE',  ( 0.000000000000000000, 0.000000000000000000, 1.000000000000000000 ) ) ;
#2165 = DIRECTION ( 'NONE',  ( 0.000000000000000000, 0.5150380749100571531, 0.8571673007021105573 ) ) ;
#2166 = ORIENTED_EDGE ( 'NONE', *, *, #5697, .T. ) ;
#2167 = CARTESIAN_POINT ( 'NONE',  ( 25.00000000000000000, 3.750000000000000000, -12.00000000000000000 ) ) ;
#2168 = CARTESIAN_POINT ( 'NONE',  ( -1.500000000000000222, -13.00000000000000533, -1.250000000000000000 ) ) ;
#2169 = CARTESIAN_POINT ( 'NONE',  ( 4.023224611898322145, -4.155232146225737111, 8.103948283277974340 ) ) ;
#2170 = ORIENTED_EDGE ( 'NONE', *, *, #382, .F. ) ;
#2171 = EDGE_CURVE ( 'NONE', #6915, #2633, #5314, .T. ) ;
#2172 = CARTESIAN_POINT ( 'NONE',  ( 1.060575238724907038E-16, -11.26794919243112680, -2.437500001365593860 ) ) ;
#2173 = CARTESIAN_POINT ( 'NONE',  ( 4.000000000000000000, -13.00000000000000533, 2.000000000000000000 ) ) ;
#2174 =( BOUNDED_SURFACE ( )  B_SPLINE_SURFACE ( 1, 2, ( 
 ( #8997, #1089, #4312, #2632, #9101, #1837, #301, #1735, #2737, #3523, #5061, #8310, #1042, #10458, #7508, #6700, #10007, #5947, #9202, #1993, #1296, #4522, #5321, #2944, #8609, #7766, #4574, #6213, #10060, #3578, #5273, #499, #3730, #2200, #5425, #7823, #6049, #1346, #2834, #6855, #10161, #7717, #8565, #7661, #554, #2784, #6962, #8666, #3782, #5999, #9304, #6906, #7011, #6804, #10215, #6162, #4363, #9418, #5212, #2150, #8460, #9255, #8512, #2045, #1246, #10266, #7606, #5370, #351, #4418, #1192, #10111, #401 ),
 ( #3626, #4471, #452, #3679, #9467, #2887, #6111, #9362, #2097, #2997, #6267, #3945, #3048, #8087, #10430, #9578, #3153, #2308, #9632, #10313, #2358, #5476, #6379, #3099, #9738, #8828, #1509, #3836, #10376, #819, #9526, #2252, #606, #7174, #5580, #7120, #655, #3889, #8038, #1570, #8879, #6481, #3203, #8715, #9690, #32, #4794, #6319, #1619, #5531, #716, #768, #1456, #4049, #8770, #4004, #7284, #4734, #3257, #7232, #4680, #7924, #7984, #2469, #10488, #7064, #6429, #2417, #5634, #4845, #5683, #1400, #4625 ) ),
 .UNSPECIFIED., .F., .F., .T. ) 
 B_SPLINE_SURFACE_WITH_KNOTS ( ( 2, 2 ),
 ( 3, 2, 2, 2, 2, 2, 2, 2, 2, 2, 2, 2, 2, 2, 2, 2, 2, 2, 2, 2, 2, 2, 2, 2, 2, 2, 2, 2, 2, 2, 2, 2, 2, 2, 2, 2, 3 ),
 ( 0.000000000000000000, 1.000000000000000000 ),
 ( 0.000000000000000000, 0.02777777777777777624, 0.05555555555555555247, 0.08333333333333332871, 0.1111111111111111049, 0.1388888888888888951, 0.1666666666666666574, 0.1944444444444444475, 0.2222222222222222099, 0.2500000000000000000, 0.2777777777777777901, 0.3055555555555555802, 0.3333333333333333148, 0.3611111111111111049, 0.3888888888888888951, 0.4166666666666666852, 0.4444444444444444198, 0.4722222222222222099, 0.5000000000000000000, 0.5277777777777777901, 0.5555555555555555802, 0.5833333333333333703, 0.6111111111111111605, 0.6388888888888888395, 0.6666666666666666297, 0.6944444444444444198, 0.7222222222222222099, 0.7500000000000000000, 0.7777777777777777901, 0.8055555555555555802, 0.8333333333333333703, 0.8611111111111111605, 0.8888888888888888395, 0.9166666666666666297, 0.9444444444444444198, 0.9722222222222222099, 1.000000000000000000 ),
 .UNSPECIFIED. ) 
 GEOMETRIC_REPRESENTATION_ITEM ( )  RATIONAL_B_SPLINE_SURFACE ( (
 ( 1.000000000000000000, 0.8660254037844387076, 1.000000000000000000, 0.8660254037844387076, 1.000000000000000000, 0.8660254037844387076, 1.000000000000000000, 0.8660254037844387076, 1.000000000000000000, 0.8660254037844387076, 1.000000000000000000, 0.8660254037844387076, 1.000000000000000000, 0.8660254037844387076, 1.000000000000000000, 0.8660254037844387076, 1.000000000000000000, 0.8660254037844387076, 1.000000000000000000, 0.8660254037844387076, 1.000000000000000000, 0.8660254037844387076, 1.000000000000000000, 0.8660254037844387076, 1.000000000000000000, 0.8660254037844387076, 1.000000000000000000, 0.8660254037844387076, 1.000000000000000000, 0.8660254037844387076, 1.000000000000000000, 0.8660254037844387076, 1.000000000000000000, 0.8660254037844387076, 1.000000000000000000, 0.8660254037844387076, 1.000000000000000000, 0.8660254037844387076, 1.000000000000000000, 0.8660254037844387076, 1.000000000000000000, 0.8660254037844387076, 1.000000000000000000, 0.8660254037844387076, 1.000000000000000000, 0.8660254037844387076, 1.000000000000000000, 0.8660254037844387076, 1.000000000000000000, 0.8660254037844387076, 1.000000000000000000, 0.8660254037844387076, 1.000000000000000000, 0.8660254037844387076, 1.000000000000000000, 0.8660254037844387076, 1.000000000000000000, 0.8660254037844387076, 1.000000000000000000, 0.8660254037844387076, 1.000000000000000000, 0.8660254037844387076, 1.000000000000000000, 0.8660254037844387076, 1.000000000000000000, 0.8660254037844387076, 1.000000000000000000, 0.8660254037844387076, 1.000000000000000000, 0.8660254037844387076, 1.000000000000000000, 0.8660254037844387076, 1.000000000000000000),
 ( 1.000000000000000000, 0.8660254037844387076, 1.000000000000000000, 0.8660254037844387076, 1.000000000000000000, 0.8660254037844387076, 1.000000000000000000, 0.8660254037844387076, 1.000000000000000000, 0.8660254037844387076, 1.000000000000000000, 0.8660254037844387076, 1.000000000000000000, 0.8660254037844387076, 1.000000000000000000, 0.8660254037844387076, 1.000000000000000000, 0.8660254037844387076, 1.000000000000000000, 0.8660254037844387076, 1.000000000000000000, 0.8660254037844387076, 1.000000000000000000, 0.8660254037844387076, 1.000000000000000000, 0.8660254037844387076, 1.000000000000000000, 0.8660254037844387076, 1.000000000000000000, 0.8660254037844387076, 1.000000000000000000, 0.8660254037844387076, 1.000000000000000000, 0.8660254037844387076, 1.000000000000000000, 0.8660254037844387076, 1.000000000000000000, 0.8660254037844387076, 1.000000000000000000, 0.8660254037844387076, 1.000000000000000000, 0.8660254037844387076, 1.000000000000000000, 0.8660254037844387076, 1.000000000000000000, 0.8660254037844387076, 1.000000000000000000, 0.8660254037844387076, 1.000000000000000000, 0.8660254037844387076, 1.000000000000000000, 0.8660254037844387076, 1.000000000000000000, 0.8660254037844387076, 1.000000000000000000, 0.8660254037844387076, 1.000000000000000000, 0.8660254037844387076, 1.000000000000000000, 0.8660254037844387076, 1.000000000000000000, 0.8660254037844387076, 1.000000000000000000, 0.8660254037844387076, 1.000000000000000000, 0.8660254037844387076, 1.000000000000000000, 0.8660254037844387076, 1.000000000000000000, 0.8660254037844387076, 1.000000000000000000, 0.8660254037844387076, 1.000000000000000000) ) ) 
 REPRESENTATION_ITEM ( '' )  SURFACE ( )  );
#2175 = LINE ( 'NONE', #7204, #5810 ) ;
#2176 = CARTESIAN_POINT ( 'NONE',  ( -4.089228379062038066, 4.089228379062022078, 13.29999999999999716 ) ) ;
#2177 = CARTESIAN_POINT ( 'NONE',  ( 0.7500000000000003331, -11.70096189432334732, -2.416666666666666963 ) ) ;
#2178 = FACE_OUTER_BOUND ( 'NONE', #9038, .T. ) ;
#2179 = CARTESIAN_POINT ( 'NONE',  ( -1.500000000000000222, -13.00000000000000533, -1.250000000000000000 ) ) ;
#2180 = DIRECTION ( 'NONE',  ( -1.000000000000000000, 0.000000000000000000, 0.000000000000000000 ) ) ;
#2181 = CARTESIAN_POINT ( 'NONE',  ( -0.7039550926810301812, -4.444597532678121965, 3.919999999999999929 ) ) ;
#2182 = AXIS2_PLACEMENT_3D ( 'NONE', #6247, #485, #5404 ) ;
#2183 = CARTESIAN_POINT ( 'NONE',  ( 8.692241771943169307E-17, -11.58044919106553294, -0.5937500006827968191 ) ) ;
#2184 = CARTESIAN_POINT ( 'NONE',  ( 4.860232935257354114, -2.576046737280751842, 10.76394828327797626 ) ) ;
#2185 = EDGE_CURVE ( 'NONE', #2333, #7985, #10306, .T. ) ;
#2186 = DIRECTION ( 'NONE',  ( 1.000000000000000000, 0.000000000000000000, 0.000000000000000000 ) ) ;
#2187 = ORIENTED_EDGE ( 'NONE', *, *, #1580, .T. ) ;
#2188 = CYLINDRICAL_SURFACE ( 'NONE', #3728, 1.249999999999993339 ) ;
#2189 = AXIS2_PLACEMENT_3D ( 'NONE', #815, #5629, #764 ) ;
#2190 = LINE ( 'NONE', #1393, #8826 ) ;
#2191 = AXIS2_PLACEMENT_3D ( 'NONE', #9273, #3497, #2012 ) ;
#2192 = CARTESIAN_POINT ( 'NONE',  ( 6.727620669667255804, -7.750000000000000000, -12.00000000000000000 ) ) ;
#2193 = LINE ( 'NONE', #2248, #2048 ) ;
#2194 = VERTEX_POINT ( 'NONE', #7758 ) ;
#2195 = VECTOR ( 'NONE', #8873, 1000.000000000000000 ) ;
#2196 = DIRECTION ( 'NONE',  ( 0.000000000000000000, 0.000000000000000000, -1.000000000000000000 ) ) ;
#2197 = DIRECTION ( 'NONE',  ( -1.000000000000000000, -0.000000000000000000, 0.000000000000000000 ) ) ;
#2198 = AXIS2_PLACEMENT_3D ( 'NONE', #6512, #3925, #1488 ) ;
#2199 = CARTESIAN_POINT ( 'NONE',  ( -3.244753828200538148, -3.119207202478392116, 0.4039482832779765498 ) ) ;
#2200 = CARTESIAN_POINT ( 'NONE',  ( -2.607672531582950546E-16, -14.41955080893447416, -1.468750000682796708 ) ) ;
#2201 = ORIENTED_EDGE ( 'NONE', *, *, #427, .F. ) ;
#2202 = ORIENTED_EDGE ( 'NONE', *, *, #2609, .T. ) ;
#2203 = CARTESIAN_POINT ( 'NONE',  ( -2.000000000000000000, 0.000000000000000000, 0.000000000000000000 ) ) ;
#2204 = VECTOR ( 'NONE', #5118, 1000.000000000000000 ) ;
#2205 = ADVANCED_FACE ( 'NONE', ( #8659 ), #5468, .F. ) ;
#2206 = CARTESIAN_POINT ( 'NONE',  ( 21.07718659994326060, -17.67146854445365989, 0.000000000000000000 ) ) ;
#2207 = VERTEX_POINT ( 'NONE', #2935 ) ;
#2208 = CARTESIAN_POINT ( 'NONE',  ( -2.542276634908081423, -5.195105386651227342, 5.056051716722023137 ) ) ;
#2209 = CARTESIAN_POINT ( 'NONE',  ( -2.000000000000012879, 15.00000000000000355, 3.999999999999986233 ) ) ;
#2210 = VERTEX_POINT ( 'NONE', #3829 ) ;
#2211 = LINE ( 'NONE', #2797, #1374 ) ;
#2212 = AXIS2_PLACEMENT_3D ( 'NONE', #6373, #9626, #8030 ) ;
#2213 = VERTEX_POINT ( 'NONE', #7816 ) ;
#2214 = SURFACE_SIDE_STYLE ('',( #674 ) ) ;
#2215 = VECTOR ( 'NONE', #10151, 1000.000000000000114 ) ;
#2216 = ORIENTED_EDGE ( 'NONE', *, *, #7634, .T. ) ;
#2217 = AXIS2_PLACEMENT_3D ( 'NONE', #4985, #2341, #4776 ) ;
#2218 = EDGE_CURVE ( 'NONE', #5749, #909, #546, .T. ) ;
#2219 = CARTESIAN_POINT ( 'NONE',  ( 27.00000000000001066, 0.000000000000000000, 0.000000000000000000 ) ) ;
#2220 = EDGE_CURVE ( 'NONE', #618, #2377, #7055, .T. ) ;
#2221 = CARTESIAN_POINT ( 'NONE',  ( 10.00000000000000000, -7.851777359434023218, 3.255701506262409506 ) ) ;
#2222 = VECTOR ( 'NONE', #1288, 1000.000000000000000 ) ;
#2223 = VERTEX_POINT ( 'NONE', #4672 ) ;
#2224 = CARTESIAN_POINT ( 'NONE',  ( 10.00000000000000000, 0.000000000000000000, 0.000000000000000000 ) ) ;
#2225 = DIRECTION ( 'NONE',  ( -1.000000000000000000, -0.000000000000000000, -0.000000000000000000 ) ) ;
#2226 = CARTESIAN_POINT ( 'NONE',  ( 2.417848759854264618, -4.940838830814695548, 8.243948283277976685 ) ) ;
#2227 = ORIENTED_EDGE ( 'NONE', *, *, #5179, .F. ) ;
#2228 = CARTESIAN_POINT ( 'NONE',  ( 1.500000000000000444, -12.13397459621556607, -2.020833334698926897 ) ) ;
#2229 = VECTOR ( 'NONE', #154, 1000.000000000000000 ) ;
#2230 = DIRECTION ( 'NONE',  ( -0.3420201433256627732, 0.9396926207859105373, 0.000000000000000000 ) ) ;
#2231 = FACE_OUTER_BOUND ( 'NONE', #10112, .T. ) ;
#2232 = EDGE_CURVE ( 'NONE', #8002, #7355, #7917, .T. ) ;
#2233 = DIRECTION ( 'NONE',  ( -1.000000000000000000, 0.000000000000000000, -0.000000000000000000 ) ) ;
#2234 = FACE_OUTER_BOUND ( 'NONE', #1528, .T. ) ;
#2235 = CARTESIAN_POINT ( 'NONE',  ( -4.000000000000000000, -13.00000000000000533, 0.000000000000000000 ) ) ;
#2236 = FACE_OUTER_BOUND ( 'NONE', #7422, .T. ) ;
#2237 = DIRECTION ( 'NONE',  ( -0.000000000000000000, -0.000000000000000000, 1.000000000000000000 ) ) ;
#2238 = CARTESIAN_POINT ( 'NONE',  ( 0.7039550926810297371, 4.444597532678122853, 2.519999999999999574 ) ) ;
#2239 = CARTESIAN_POINT ( 'NONE',  ( 8.692241771943169307E-17, -11.58044919106553294, -0.09375000068279677745 ) ) ;
#2240 = CARTESIAN_POINT ( 'NONE',  ( -4.860232935257354114, 2.576046737280751842, 6.563948283277975193 ) ) ;
#2241 = CARTESIAN_POINT ( 'NONE',  ( 0.000000000000000000, -13.00000000000000533, -3.000000000000000000 ) ) ;
#2242 = ORIENTED_EDGE ( 'NONE', *, *, #721, .T. ) ;
#2243 = APPLICATION_PROTOCOL_DEFINITION ( 'draft international standard', 'automotive_design', 1998, #4179 ) ;
#2244 = CARTESIAN_POINT ( 'NONE',  ( -1.500000000000002665, -13.86602540378444282, -2.270833334698926453 ) ) ;
#2245 = CARTESIAN_POINT ( 'NONE',  ( 0.4444353696672553311, 3.750000000000000000, -12.00000000000000000 ) ) ;
#2246 = LINE ( 'NONE', #445, #2395 ) ;
#2247 = DIRECTION ( 'NONE',  ( -1.000000000000000000, -0.000000000000000000, -0.000000000000000000 ) ) ;
#2248 = CARTESIAN_POINT ( 'NONE',  ( 6.727620669667255804, 3.750000000000000000, 0.000000000000000000 ) ) ;
#2249 = ORIENTED_EDGE ( 'NONE', *, *, #9736, .T. ) ;
#2250 = DIRECTION ( 'NONE',  ( 0.000000000000000000, -0.5000000000000013323, -0.8660254037844378194 ) ) ;
#2251 = CARTESIAN_POINT ( 'NONE',  ( 4.444597532678119300, 0.7039550926810472786, 11.47999999999999865 ) ) ;
#2252 = CARTESIAN_POINT ( 'NONE',  ( -1.500000000000000666, -13.86602540378444459, -1.708333333333333481 ) ) ;
#2253 = ORIENTED_EDGE ( 'NONE', *, *, #6017, .T. ) ;
#2254 = EDGE_CURVE ( 'NONE', #2333, #3169, #4079, .T. ) ;
#2255 = VERTEX_POINT ( 'NONE', #4977 ) ;
#2256 = DIRECTION ( 'NONE',  ( 0.3420201433256627732, 0.9396926207859105373, 0.000000000000000000 ) ) ;
#2257 = CIRCLE ( 'NONE', #8024, 2.000000000000000000 ) ;
#2258 = EDGE_CURVE ( 'NONE', #9806, #9585, #1599, .T. ) ;
#2259 = VERTEX_POINT ( 'NONE', #9013 ) ;
#2260 = CARTESIAN_POINT ( 'NONE',  ( -5.726445515403654873, 0.8124729078101847746, 8.416051716722021681 ) ) ;
#2261 = CARTESIAN_POINT ( 'NONE',  ( 2.625446233515515537, 5.152728359536502545, 13.85999999999999766 ) ) ;
#2262 = ORIENTED_EDGE ( 'NONE', *, *, #5783, .F. ) ;
#2263 = CARTESIAN_POINT ( 'NONE',  ( 10.00000000000000000, 0.000000000000000000, 0.000000000000000000 ) ) ;
#2264 = CARTESIAN_POINT ( 'NONE',  ( 3.826313983664925811, 3.951860609387098044, 14.99605171672202175 ) ) ;
#2265 = EDGE_CURVE ( 'NONE', #4339, #8766, #9683, .T. ) ;
#2266 = VERTEX_POINT ( 'NONE', #3235 ) ;
#2267 =( GEOMETRIC_REPRESENTATION_CONTEXT ( 3 ) GLOBAL_UNCERTAINTY_ASSIGNED_CONTEXT ( ( #4377 ) ) GLOBAL_UNIT_ASSIGNED_CONTEXT ( ( #8113, #4925, #8273 ) ) REPRESENTATION_CONTEXT ( 'NONE', 'WORKASPACE' ) );
#2268 = ORIENTED_EDGE ( 'NONE', *, *, #734, .T. ) ;
#2269 = CARTESIAN_POINT ( 'NONE',  ( -29.99999999999998934, 34.99999999999999289, 9.000000000000000000 ) ) ;
#2270 = CARTESIAN_POINT ( 'NONE',  ( 30.00000000000001066, 1.959434878635752904E-16, 1.599999999999986766 ) ) ;
#2271 = ORIENTED_EDGE ( 'NONE', *, *, #9419, .F. ) ;
#2272 = LINE ( 'NONE', #8584, #5572 ) ;
#2273 = CARTESIAN_POINT ( 'NONE',  ( 0.000000000000000000, 6.000000000000000000, 0.000000000000000000 ) ) ;
#2274 = CARTESIAN_POINT ( 'NONE',  ( 4.860232935257354114, -2.576046737280751842, 5.163948283277975726 ) ) ;
#2276 = VERTEX_POINT ( 'NONE', #6620 ) ;
#2275 = CIRCLE ( 'NONE', #2085, 8.500000000000000000 ) ;
#2277 = CARTESIAN_POINT ( 'NONE',  ( 9.869213319667256457, -7.750000000000000000, 0.000000000000000000 ) ) ;
#2278 = EDGE_CURVE ( 'NONE', #7564, #10476, #6459, .T. ) ;
#2279 = EDGE_CURVE ( 'NONE', #9635, #6751, #7210, .T. ) ;
#2280 = LINE ( 'NONE', #3973, #9051 ) ;
#2281 = ORIENTED_EDGE ( 'NONE', *, *, #7853, .F. ) ;
#2282 = CARTESIAN_POINT ( 'NONE',  ( -0.7500000000000007772, -14.29903810567666156, -0.7291666680322601568 ) ) ;
#2283 = CARTESIAN_POINT ( 'NONE',  ( 8.000000000000001776, -1.179494851233864106, -6.136676046192498291 ) ) ;
#2284 = CARTESIAN_POINT ( 'NONE',  ( -29.99999999999998934, 1.959434878635763751E-16, -1.599999999999998979 ) ) ;
#2285 = DIRECTION ( 'NONE',  ( -1.000000000000000000, -0.000000000000000000, -0.000000000000000000 ) ) ;
#2286 = AXIS2_PLACEMENT_3D ( 'NONE', #9068, #6664, #9012 ) ;
#2287 = CARTESIAN_POINT ( 'NONE',  ( -0.6146835312499998594, -11.93533689329915326, -2.677083334016129967 ) ) ;
#2288 = CARTESIAN_POINT ( 'NONE',  ( -4.444597532678119300, -0.7039550926810477227, 10.07999999999999829 ) ) ;
#2289 = CARTESIAN_POINT ( 'NONE',  ( -2.607672531582950546E-16, -14.41955080893447416, -1.468750000682796708 ) ) ;
#2290 = PRODUCT_DEFINITION_FORMATION_WITH_SPECIFIED_SOURCE ( 'ANY', '', #10292, .NOT_KNOWN. ) ;
#2291 = ADVANCED_FACE ( 'NONE', ( #10464 ), #5710, .F. ) ;
#2292 = CARTESIAN_POINT ( 'NONE',  ( 3.951860609387084722, 3.826313983664940022, 13.00394828327797470 ) ) ;
#2293 = FACE_OUTER_BOUND ( 'NONE', #9810, .T. ) ;
#2294 = VECTOR ( 'NONE', #9909, 1000.000000000000000 ) ;
#2295 = EDGE_LOOP ( 'NONE', ( #2916, #6667, #9251, #5439 ) ) ;
#2296 = SHAPE_DEFINITION_REPRESENTATION ( #4871, #1027 ) ;
#2297 = CARTESIAN_POINT ( 'NONE',  ( 1.272613240716556016, 6.025400000000000311, -12.00000000000000000 ) ) ;
#2298 = DIRECTION ( 'NONE',  ( 0.000000000000000000, -1.000000000000000000, 0.000000000000000000 ) ) ;
#2299 = ORIENTED_EDGE ( 'NONE', *, *, #784, .T. ) ;
#2300 = CARTESIAN_POINT ( 'NONE',  ( 27.00000000000001066, 1.959434878635756602E-16, 1.599999999999992983 ) ) ;
#2301 = CARTESIAN_POINT ( 'NONE',  ( -1.500000000000000222, -13.00000000000000533, -1.750000000000000000 ) ) ;
#2302 = VERTEX_POINT ( 'NONE', #3390 ) ;
#2303 = SURFACE_STYLE_USAGE ( .BOTH. , #7008 ) ;
#2304 = CARTESIAN_POINT ( 'NONE',  ( 0.000000000000000000, 1.478016689125442484, -1.626303258728256651E-15 ) ) ;
#2305 = EDGE_CURVE ( 'NONE', #8379, #4528, #956, .T. ) ;
#2306 = CARTESIAN_POINT ( 'NONE',  ( 2.148092372876330369, 4.215868657802593233, 11.05999999999999872 ) ) ;
#2307 = UNCERTAINTY_MEASURE_WITH_UNIT (LENGTH_MEASURE( 1.000000000000000082E-05 ), #2584, 'distance_accuracy_value', 'NONE');
#2308 = CARTESIAN_POINT ( 'NONE',  ( -1.500000000000000000, -12.13397459621556607, -2.291666666666666963 ) ) ;
#2309 = ORIENTED_EDGE ( 'NONE', *, *, #10325, .T. ) ;
#2310 = VERTEX_POINT ( 'NONE', #1648 ) ;
#2311 = CARTESIAN_POINT ( 'NONE',  ( 1.500000000000000222, -12.13397459621556784, -0.9583333333333337034 ) ) ;
#2312 = ORIENTED_EDGE ( 'NONE', *, *, #6038, .T. ) ;
#2313 = CARTESIAN_POINT ( 'NONE',  ( -4.049832306626335310, 1.963858260114700327, 8.556051716722022249 ) ) ;
#2314 = LINE ( 'NONE', #5537, #1333 ) ;
#2315 = DIRECTION ( 'NONE',  ( -0.000000000000000000, 1.000000000000000000, -0.000000000000000000 ) ) ;
#2316 = ORIENTED_EDGE ( 'NONE', *, *, #2232, .F. ) ;
#2317 = DIRECTION ( 'NONE',  ( -1.000000000000000000, -0.000000000000000000, -0.000000000000000000 ) ) ;
#2318 = CARTESIAN_POINT ( 'NONE',  ( 0.9968613283357860011, -5.697241258616382531, 13.17605171672201969 ) ) ;
#2319 = EDGE_LOOP ( 'NONE', ( #7682, #7519, #8207, #1253 ) ) ;
#2320 = EDGE_LOOP ( 'NONE', ( #3515, #662, #3143, #3332 ) ) ;
#2321 = CARTESIAN_POINT ( 'NONE',  ( 30.00000000000001066, -31.99999999999998579, 5.999999999999999112 ) ) ;
#2322 = CIRCLE ( 'NONE', #3922, 1.999999999999997780 ) ;
#2323 = CARTESIAN_POINT ( 'NONE',  ( 0.000000000000000000, 6.000000000000000000, 0.000000000000000000 ) ) ;
#2324 = ORIENTED_EDGE ( 'NONE', *, *, #1943, .F. ) ;
#2325 = FACE_OUTER_BOUND ( 'NONE', #3648, .T. ) ;
#2326 = EDGE_CURVE ( 'NONE', #5471, #9996, #6564, .T. ) ;
#2327 = DIRECTION ( 'NONE',  ( -0.000000000000000000, 0.000000000000000000, -1.000000000000000000 ) ) ;
#2328 = CARTESIAN_POINT ( 'NONE',  ( 5.195105386651219348, 2.542276634908100075, 1.943948283277976419 ) ) ;
#2329 = ORIENTED_EDGE ( 'NONE', *, *, #2530, .T. ) ;
#2330 = CARTESIAN_POINT ( 'NONE',  ( 8.692241771943169307E-17, -11.58044919106553294, -2.593750000682796486 ) ) ;
#2331 = DIRECTION ( 'NONE',  ( 1.000000000000000000, 0.000000000000000000, 0.000000000000000000 ) ) ;
#2332 = CARTESIAN_POINT ( 'NONE',  ( 5.999999999999999112, 26.99999999999999289, -4.000000000000000000 ) ) ;
#2333 = VERTEX_POINT ( 'NONE', #9816 ) ;
#2334 = CARTESIAN_POINT ( 'NONE',  ( -1.500000000000003775, -13.86602540378444104, -0.7708333346989270085 ) ) ;
#2335 = CARTESIAN_POINT ( 'NONE',  ( -2.000000000000024425, 15.00000000000000355, 5.999999999999987566 ) ) ;
#2336 = CARTESIAN_POINT ( 'NONE',  ( -15.00000000000000000, 19.99999999999999645, -9.000000000000000000 ) ) ;
#2337 = CARTESIAN_POINT ( 'NONE',  ( 9.869213319667256457, 3.750000000000000000, -12.00000000000000000 ) ) ;
#2338 = ADVANCED_FACE ( 'NONE', ( #850 ), #4028, .F. ) ;
#2339 = LINE ( 'NONE', #5616, #4545 ) ;
#2340 = CARTESIAN_POINT ( 'NONE',  ( -4.444597532678119300, -0.7039550926810477227, 4.479999999999999538 ) ) ;
#2341 = DIRECTION ( 'NONE',  ( 1.000000000000000000, 0.000000000000000000, 0.000000000000000000 ) ) ;
#2342 = CARTESIAN_POINT ( 'NONE',  ( 0.8124729078102063129, -5.726445515403652209, 5.583948283277975655 ) ) ;
#2343 = CYLINDRICAL_SURFACE ( 'NONE', #3104, 3.000000000000000000 ) ;
#2344 = VERTEX_POINT ( 'NONE', #58 ) ;
#2345 = ITEM_DEFINED_TRANSFORMATION ( 'NONE', 'NONE', #1274,  #2101 ) ;
#2346 = CARTESIAN_POINT ( 'NONE',  ( -5.711843387010019590, 0.9046671180729746187, 1.819999999999999618 ) ) ;
#2347 = CARTESIAN_POINT ( 'NONE',  ( -1.500000000000000666, -13.86602540378444637, -1.770833334698926897 ) ) ;
#2348 = ADVANCED_FACE ( 'NONE', ( #7317 ), #8908, .F. ) ;
#2349 = ORIENTED_EDGE ( 'NONE', *, *, #2486, .T. ) ;
#2350 = CARTESIAN_POINT ( 'NONE',  ( 0.4444353696672553311, -7.750000000000000000, -12.00000000000000000 ) ) ;
#2351 = ADVANCED_FACE ( 'NONE', ( #1699 ), #5815, .F. ) ;
#2352 = CARTESIAN_POINT ( 'NONE',  ( 1.499999999999999778, -13.86602540378444637, -1.541666666666666963 ) ) ;
#2353 = DIRECTION ( 'NONE',  ( 0.000000000000000000, 0.000000000000000000, -1.000000000000000000 ) ) ;
#2354 =( NAMED_UNIT ( * ) PLANE_ANGLE_UNIT ( ) SI_UNIT ( $, .RADIAN. ) );
#2355 = CARTESIAN_POINT ( 'NONE',  ( 16.15239861966725599, -7.750000000000000000, -12.00000000000000000 ) ) ;
#2356 = CARTESIAN_POINT ( 'NONE',  ( -0.7401821875142701179, 4.673326407553649808, 7.979999999999999538 ) ) ;
#2357 = APPLICATION_CONTEXT ( 'automotive_design' ) ;
#2358 = CARTESIAN_POINT ( 'NONE',  ( -0.7500000000000007772, -14.29903810567666156, -2.166666666666666519 ) ) ;
#2359 = VECTOR ( 'NONE', #8860, 1000.000000000000000 ) ;
#2360 = EDGE_LOOP ( 'NONE', ( #4693, #6871 ) ) ;
#2361 = EDGE_LOOP ( 'NONE', ( #7769, #7206, #1682, #7238 ) ) ;
#2362 = EDGE_CURVE ( 'NONE', #7675, #9850, #7807, .T. ) ;
#2363 = LINE ( 'NONE', #2421, #5258 ) ;
#2364 = FACE_OUTER_BOUND ( 'NONE', #153, .T. ) ;
#2365 = ORIENTED_EDGE ( 'NONE', *, *, #9195, .T. ) ;
#2366 = CARTESIAN_POINT ( 'NONE',  ( 10.00000000000000000, 8.265874651078044977, -1.981241088980697729 ) ) ;
#2367 = ORIENTED_EDGE ( 'NONE', *, *, #7400, .T. ) ;
#2368 = CIRCLE ( 'NONE', #2191, 1.249999999999988898 ) ;
#2369 = DIRECTION ( 'NONE',  ( -1.000000000000000000, -0.000000000000000000, 0.000000000000000000 ) ) ;
#2370 = CARTESIAN_POINT ( 'NONE',  ( -5.110351332421769754, -2.708615832122969191, 10.93605171672202125 ) ) ;
#2371 = ORIENTED_EDGE ( 'NONE', *, *, #10190, .T. ) ;
#2372 = SURFACE_SIDE_STYLE ('',( #5018 ) ) ;
#2373 = CIRCLE ( 'NONE', #4055, 3.000000000000000000 ) ;
#2374 = CARTESIAN_POINT ( 'NONE',  ( -2.000000000000001776, 0.000000000000000000, 2.000000000000000000 ) ) ;
#2375 = CIRCLE ( 'NONE', #10336, 8.500000000000000000 ) ;
#2376 = DIRECTION ( 'NONE',  ( 0.000000000000000000, 0.000000000000000000, -1.000000000000000000 ) ) ;
#2377 = VERTEX_POINT ( 'NONE', #2392 ) ;
#2378 = CARTESIAN_POINT ( 'NONE',  ( -0.8603895577212598011, -5.432285873273260179, 6.719999999999999751 ) ) ;
#2379 = DIRECTION ( 'NONE',  ( -1.000000000000000000, 0.000000000000000000, -0.000000000000000000 ) ) ;
#2380 = CARTESIAN_POINT ( 'NONE',  ( -4.900535883036028828, 2.496947748567499126, 1.959999999999999964 ) ) ;
#2381 = ORIENTED_EDGE ( 'NONE', *, *, #5192, .F. ) ;
#2382 = AXIS2_PLACEMENT_3D ( 'NONE', #945, #5065, #1048 ) ;
#2383 = CARTESIAN_POINT ( 'NONE',  ( 0.7500000000000003331, -11.70096189432334732, -0.4791666680322602123 ) ) ;
#2384 = VECTOR ( 'NONE', #9630, 1000.000000000000000 ) ;
#2385 = CIRCLE ( 'NONE', #1200, 8.500000000000000000 ) ;
#2386 =( LENGTH_UNIT ( ) NAMED_UNIT ( * ) SI_UNIT ( .MILLI., .METRE. ) );
#2387 = ORIENTED_EDGE ( 'NONE', *, *, #4483, .F. ) ;
#2388 = VECTOR ( 'NONE', #7826, 1000.000000000000000 ) ;
#2389 = EDGE_CURVE ( 'NONE', #9588, #4358, #3181, .T. ) ;
#2390 = DIRECTION ( 'NONE',  ( -1.000000000000000000, 0.000000000000000000, 0.000000000000000000 ) ) ;
#2391 = VECTOR ( 'NONE', #3951, 1000.000000000000000 ) ;
#2392 = CARTESIAN_POINT ( 'NONE',  ( 14.44459485323380576, 6.000000000000000000, 0.000000000000000000 ) ) ;
#2393 = FACE_OUTER_BOUND ( 'NONE', #8936, .T. ) ;
#2394 = DIRECTION ( 'NONE',  ( 0.9396926207859105373, 0.3420201433256627732, 0.000000000000000000 ) ) ;
#2395 = VECTOR ( 'NONE', #7709, 1000.000000000000000 ) ;
#2396 = DIRECTION ( 'NONE',  ( -1.000000000000000000, -0.000000000000000000, -0.000000000000000000 ) ) ;
#2397 = CARTESIAN_POINT ( 'NONE',  ( -0.7401821875142701179, 4.673326407553649808, 5.179999999999999716 ) ) ;
#2398 = VERTEX_POINT ( 'NONE', #5613 ) ;
#2399 = CARTESIAN_POINT ( 'NONE',  ( 8.692241771943169307E-17, -11.58044919106553294, -1.218750000682796930 ) ) ;
#2400 = CIRCLE ( 'NONE', #1041, 1.599999999999986766 ) ;
#2401 = CARTESIAN_POINT ( 'NONE',  ( 2.708615832122949652, 5.110351332421781301, 10.06394828327797519 ) ) ;
#2402 = CARTESIAN_POINT ( 'NONE',  ( -2.000000000000000000, 8.265874651078018331, 1.981241088980807419 ) ) ;
#2403 = EDGE_CURVE ( 'NONE', #6339, #1944, #112, .T. ) ;
#2404 = EDGE_LOOP ( 'NONE', ( #2281, #9067 ) ) ;
#2405 = APPLICATION_PROTOCOL_DEFINITION ( 'draft international standard', 'automotive_design', 1998, #6338 ) ;
#2406 = CARTESIAN_POINT ( 'NONE',  ( 2.496947748567516889, -4.900535883036019946, 0.8399999999999999689 ) ) ;
#2407 = DIRECTION ( 'NONE',  ( -1.156482317317871478E-16, 1.000000000000000000, 0.000000000000000000 ) ) ;
#2408 = ORIENTED_EDGE ( 'NONE', *, *, #468, .F. ) ;
#2409 = DIRECTION ( 'NONE',  ( -1.000000000000000000, -0.000000000000000000, -0.000000000000000000 ) ) ;
#2410 = DIRECTION ( 'NONE',  ( 0.000000000000000000, 0.000000000000000000, 1.000000000000000000 ) ) ;
#2411 = DIRECTION ( 'NONE',  ( 0.000000000000000000, 0.000000000000000000, -1.000000000000000000 ) ) ;
#2412 = CARTESIAN_POINT ( 'NONE',  ( 10.00000000000000000, -1.179494851233864106, -6.136676046192498291 ) ) ;
#2413 = CARTESIAN_POINT ( 'NONE',  ( 10.00000000000000000, 8.357095590591340439, 1.552080310331536372 ) ) ;
#2414 = CARTESIAN_POINT ( 'NONE',  ( 4.658724279160018966, -0.8323763977770426425, -0.5760517167220230439 ) ) ;
#2415 = PRODUCT_DEFINITION_CONTEXT ( 'detailed design', #3097, 'design' ) ;
#2416 = EDGE_CURVE ( 'NONE', #6924, #6457, #2547, .T. ) ;
#2417 = CARTESIAN_POINT ( 'NONE',  ( -1.500000000000000666, -13.86602540378444459, -0.2083333333333333703 ) ) ;
#2418 = EDGE_CURVE ( 'NONE', #3874, #7594, #4769, .T. ) ;
#2419 = VERTEX_POINT ( 'NONE', #9116 ) ;
#2420 = VERTEX_POINT ( 'NONE', #3786 ) ;
#2421 = CARTESIAN_POINT ( 'NONE',  ( 0.000000000000000000, -10.00000000000000000, -12.00000000000000000 ) ) ;
#2422 = CARTESIAN_POINT ( 'NONE',  ( 7.054542135639013677E-15, -28.99999999999999289, 0.000000000000000000 ) ) ;
#2423 = ORIENTED_EDGE ( 'NONE', *, *, #1850, .T. ) ;
#2424 = CARTESIAN_POINT ( 'NONE',  ( -2.148092372876330813, -4.215868657802594122, 1.259999999999999787 ) ) ;
#2425 = CARTESIAN_POINT ( 'NONE',  ( 0.000000000000000000, 0.000000000000000000, -12.00000000000000000 ) ) ;
#2426 = VERTEX_POINT ( 'NONE', #3631 ) ;
#2427 = CARTESIAN_POINT ( 'NONE',  ( -4.173491630687863108, -2.231261971483782691, 2.536051716722023119 ) ) ;
#2428 = EDGE_CURVE ( 'NONE', #9050, #1645, #1804, .T. ) ;
#2429 = ORIENTED_EDGE ( 'NONE', *, *, #8334, .F. ) ;
#2430 = PRESENTATION_STYLE_ASSIGNMENT (( #9052 ) ) ;
#2431 = AXIS2_PLACEMENT_3D ( 'NONE', #430, #3659, #4601 ) ;
#2432 = LINE ( 'NONE', #4756, #9583 ) ;
#2433 = CARTESIAN_POINT ( 'NONE',  ( -1.500000000000000222, -13.00000000000000533, -3.000000000000000000 ) ) ;
#2434 = ORIENTED_EDGE ( 'NONE', *, *, #4300, .T. ) ;
#2435 = CARTESIAN_POINT ( 'NONE',  ( 5.711843387010018702, -0.9046671180729751738, 0.4199999999999999289 ) ) ;
#2436 = CARTESIAN_POINT ( 'NONE',  ( -2.000000000000000000, -7.063614741696270016, 3.730353617970412206 ) ) ;
#2437 = CARTESIAN_POINT ( 'NONE',  ( 0.8124729078102063129, -5.726445515403652209, 11.18394828327797441 ) ) ;
#2438 = EDGE_LOOP ( 'NONE', ( #782, #1156, #10037, #224 ) ) ;
#2439 = CARTESIAN_POINT ( 'NONE',  ( 1.500000000000000222, -13.00000000000000533, -0.06250000136559345776 ) ) ;
#2440 = CONTEXT_DEPENDENT_SHAPE_REPRESENTATION ( #6066, #3606 ) ;
#2441 = CIRCLE ( 'NONE', #9892, 2.000000000000003553 ) ;
#2442 = ADVANCED_FACE ( 'NONE', ( #2949 ), #5218, .F. ) ;
#2443 = FILL_AREA_STYLE_COLOUR ( '', #7171 ) ;
#2444 = VERTEX_POINT ( 'NONE', #7478 ) ;
#2445 = DIRECTION ( 'NONE',  ( 1.000000000000000000, 0.000000000000000000, 0.000000000000000000 ) ) ;
#2446 = DIRECTION ( 'NONE',  ( -0.8660254037844397068, -0.000000000000000000, 0.4999999999999983347 ) ) ;
#2447 = CARTESIAN_POINT ( 'NONE',  ( 20.12216914071655793, 6.025400000000000311, -12.00000000000000000 ) ) ;
#2448 = VECTOR ( 'NONE', #2124, 1000.000000000000000 ) ;
#2449 = DIRECTION ( 'NONE',  ( -1.000000000000000000, -0.000000000000000000, -0.000000000000000000 ) ) ;
#2450 = DIRECTION ( 'NONE',  ( -0.000000000000000000, -1.000000000000000000, -0.000000000000000000 ) ) ;
#2451 = CARTESIAN_POINT ( 'NONE',  ( -4.658724279160018078, 0.8323763977770419764, 3.623948283277976135 ) ) ;
#2452 = ORIENTED_EDGE ( 'NONE', *, *, #3400, .T. ) ;
#2453 = CARTESIAN_POINT ( 'NONE',  ( 0.6146835312500001924, -11.93533689329915326, -0.7604166673494633377 ) ) ;
#2454 = CARTESIAN_POINT ( 'NONE',  ( -2.496947748567517333, 4.900535883036019058, 7.839999999999999858 ) ) ;
#2455 = DIRECTION ( 'NONE',  ( 0.000000000000000000, 0.000000000000000000, -1.000000000000000000 ) ) ;
#2456 = PRODUCT_CONTEXT ( 'NONE', #10355, 'mechanical' ) ;
#2457 = EDGE_CURVE ( 'NONE', #2653, #1211, #2839, .T. ) ;
#2458 = CARTESIAN_POINT ( 'NONE',  ( 5.152728359536493663, 2.625446233515533745, 2.939999999999999503 ) ) ;
#2459 = VECTOR ( 'NONE', #2233, 1000.000000000000000 ) ;
#2460 = CARTESIAN_POINT ( 'NONE',  ( 21.07718659994326060, 13.67146854445365811, 0.000000000000000000 ) ) ;
#2461 = CARTESIAN_POINT ( 'NONE',  ( 10.00000000000000000, -3.573533178329545645, -5.126388750707257635 ) ) ;
#2462 = DIRECTION ( 'NONE',  ( 0.000000000000000000, 0.000000000000000000, 1.000000000000000000 ) ) ;
#2463 = LINE ( 'NONE', #5678, #8463 ) ;
#2464 = ADVANCED_FACE ( 'NONE', ( #4525 ), #8276, .F. ) ;
#2465 = DIRECTION ( 'NONE',  ( -1.000000000000000000, 0.000000000000000000, 0.000000000000000000 ) ) ;
#2466 = CARTESIAN_POINT ( 'NONE',  ( -2.000000000000012879, 15.00000000000000355, 3.999999999999986233 ) ) ;
#2467 = VECTOR ( 'NONE', #5545, 1000.000000000000000 ) ;
#2468 = CARTESIAN_POINT ( 'NONE',  ( 3.244753828200538148, 3.119207202478391672, 4.603948283277976117 ) ) ;
#2469 = CARTESIAN_POINT ( 'NONE',  ( 1.060575238724907038E-16, -11.26794919243112680, -0.3750000000000003886 ) ) ;
#2470 = EDGE_LOOP ( 'NONE', ( #2367, #5647, #3284, #2016 ) ) ;
#2471 = ORIENTED_EDGE ( 'NONE', *, *, #4014, .F. ) ;
#2472 = CARTESIAN_POINT ( 'NONE',  ( 4.000000000000000888, 1.106368468154538931, -8.427689411260562480 ) ) ;
#2473 = LINE ( 'NONE', #243, #3233 ) ;
#2474 = ORIENTED_EDGE ( 'NONE', *, *, #2136, .F. ) ;
#2475 = CIRCLE ( 'NONE', #4659, 3.000000000000000000 ) ;
#2476 = CARTESIAN_POINT ( 'NONE',  ( -4.673326407553653361, 0.7401821875142517992, 4.620000000000000107 ) ) ;
#2477 = EDGE_CURVE ( 'NONE', #7886, #9192, #1719, .T. ) ;
#2478 = PLANE ( 'NONE',  #6428 ) ;
#2479 = EDGE_LOOP ( 'NONE', ( #4219, #4915, #9845, #10237 ) ) ;
#2480 = CARTESIAN_POINT ( 'NONE',  ( 3.119207202478379681, 3.244753828200549695, 9.396051716722022107 ) ) ;
#2481 = VECTOR ( 'NONE', #5979, 1000.000000000000000 ) ;
#2482 = ORIENTED_EDGE ( 'NONE', *, *, #6236, .F. ) ;
#2483 = AXIS2_PLACEMENT_3D ( 'NONE', #2023, #284, #1125 ) ;
#2484 = CARTESIAN_POINT ( 'NONE',  ( -2.000000000000000000, 6.226349476952025341, 0.5315761383463611933 ) ) ;
#2485 = ORIENTED_EDGE ( 'NONE', *, *, #1673, .T. ) ;
#2486 = EDGE_CURVE ( 'NONE', #8955, #9594, #5278, .T. ) ;
#2487 = CARTESIAN_POINT ( 'NONE',  ( 3.889087296526005488, 3.889087296526018811, 2.799999999999999378 ) ) ;
#2488 = EDGE_CURVE ( 'NONE', #9102, #5109, #407, .T. ) ;
#2489 = FACE_OUTER_BOUND ( 'NONE', #9905, .T. ) ;
#2490 = CARTESIAN_POINT ( 'NONE',  ( 4.900535883036028828, -2.496947748567499126, 3.359999999999999876 ) ) ;
#2491 = ORIENTED_EDGE ( 'NONE', *, *, #9814, .T. ) ;
#2492 = CARTESIAN_POINT ( 'NONE',  ( 1.500000000000000444, -12.13397459621556607, -1.020833334698926897 ) ) ;
#2493 = FILL_AREA_STYLE ('',( #2443 ) ) ;
#2494 = EDGE_LOOP ( 'NONE', ( #8137, #10442, #1297, #900 ) ) ;
#2495 = CARTESIAN_POINT ( 'NONE',  ( 1.229367062500000163, -13.00000000000000533, 0.2812499993172035695 ) ) ;
#2496 = CARTESIAN_POINT ( 'NONE',  ( -2.000000000000000000, 0.000000000000000000, 0.000000000000000000 ) ) ;
#2497 = DIRECTION ( 'NONE',  ( 1.000000000000000000, 0.000000000000000000, 0.000000000000000000 ) ) ;
#2498 = EDGE_CURVE ( 'NONE', #1349, #2589, #1002, .T. ) ;
#2499 = FACE_OUTER_BOUND ( 'NONE', #1114, .T. ) ;
#2500 = CARTESIAN_POINT ( 'NONE',  ( 9.869213319667256457, -7.750000000000000000, -12.00000000000000000 ) ) ;
#2501 = CARTESIAN_POINT ( 'NONE',  ( 0.7916369971161419938, 4.430710083317576320, 1.523948283277976268 ) ) ;
#2502 = ORIENTED_EDGE ( 'NONE', *, *, #6178, .T. ) ;
#2503 = FACE_BOUND ( 'NONE', #5490, .T. ) ;
#2504 = CARTESIAN_POINT ( 'NONE',  ( 5.711843387010018702, -0.9046671180729751738, 0.4199999999999999289 ) ) ;
#2505 = CARTESIAN_POINT ( 'NONE',  ( 15.00000000000000000, 19.99999999999999645, 6.000000000000000000 ) ) ;
#2506 = CYLINDRICAL_SURFACE ( 'NONE', #6507, 3.000000000000000000 ) ;
#2507 = DIRECTION ( 'NONE',  ( 0.000000000000000000, 1.000000000000000000, 0.000000000000000000 ) ) ;
#2508 = DIRECTION ( 'NONE',  ( 0.000000000000000000, 0.000000000000000000, -1.000000000000000000 ) ) ;
#2509 = CARTESIAN_POINT ( 'NONE',  ( 3.586028019667255595, 3.750000000000000000, -12.00000000000000000 ) ) ;
#2510 = PRODUCT_DEFINITION_SHAPE ( 'NONE', 'NONE',  #10499 ) ;
#2511 = LINE ( 'NONE', #918, #2195 ) ;
#2512 = CARTESIAN_POINT ( 'NONE',  ( 0.8323763977770604061, -4.658724279160015413, 4.776051716722021112 ) ) ;
#2513 = EDGE_CURVE ( 'NONE', #5181, #7025, #6115, .T. ) ;
#2514 = CARTESIAN_POINT ( 'NONE',  ( 13.01080596966725622, 3.750000000000000000, 0.000000000000000000 ) ) ;
#2515 = CARTESIAN_POINT ( 'NONE',  ( 4.658724279160018966, -0.8323763977770426425, 7.823948283277974980 ) ) ;
#2516 = LINE ( 'NONE', #5002, #3607 ) ;
#2517 = ORIENTED_EDGE ( 'NONE', *, *, #3917, .T. ) ;
#2518 = ORIENTED_EDGE ( 'NONE', *, *, #4350, .F. ) ;
#2519 = CYLINDRICAL_SURFACE ( 'NONE', #7474, 1.500000000000000222 ) ;
#2520 = PLANE ( 'NONE',  #6097 ) ;
#2521 = ORIENTED_EDGE ( 'NONE', *, *, #6093, .F. ) ;
#2522 = CARTESIAN_POINT ( 'NONE',  ( -2.148092372876330813, -4.215868657802594122, 4.059999999999999609 ) ) ;
#2523 = CARTESIAN_POINT ( 'NONE',  ( 0.000000000000000000, 0.000000000000000000, -12.00000000000000000 ) ) ;
#2524 = ORIENTED_EDGE ( 'NONE', *, *, #9868, .T. ) ;
#2525 = VECTOR ( 'NONE', #3132, 1000.000000000000000 ) ;
#2526 = CARTESIAN_POINT ( 'NONE',  ( -4.049832306626335310, 1.963858260114700327, 11.35605171672202296 ) ) ;
#2527 = CARTESIAN_POINT ( 'NONE',  ( 0.000000000000000000, 0.000000000000000000, 6.999999999999999112 ) ) ;
#2528 = VERTEX_POINT ( 'NONE', #3001 ) ;
#2529 = FILL_AREA_STYLE_COLOUR ( '', #1263 ) ;
#2530 = EDGE_CURVE ( 'NONE', #5853, #5625, #3442, .T. ) ;
#2531 = ORIENTED_EDGE ( 'NONE', *, *, #6003, .F. ) ;
#2532 = LINE ( 'NONE', #5020, #5671 ) ;
#2533 = AXIS2_PLACEMENT_3D ( 'NONE', #9412, #713, #3148 ) ;
#2534 = EDGE_LOOP ( 'NONE', ( #3784, #7396, #7123 ) ) ;
#2535 = AXIS2_PLACEMENT_3D ( 'NONE', #3543, #1912, #9329 ) ;
#2536 = CARTESIAN_POINT ( 'NONE',  ( -4.089228379062038066, 4.089228379062021190, 4.900000000000000355 ) ) ;
#2537 = CARTESIAN_POINT ( 'NONE',  ( -0.8603895577212598011, -5.432285873273260179, 6.719999999999999751 ) ) ;
#2538 = CARTESIAN_POINT ( 'NONE',  ( -2.417848759854264618, 4.940838830814694660, 9.643948283277975264 ) ) ;
#2539 = EDGE_LOOP ( 'NONE', ( #2163, #8454, #6390, #2826 ) ) ;
#2540 = AXIS2_PLACEMENT_3D ( 'NONE', #763, #3997, #2353 ) ;
#2541 = CARTESIAN_POINT ( 'NONE',  ( 1.229367062499999719, -13.70977540446724063, -0.7604166673494633377 ) ) ;
#2542 = VECTOR ( 'NONE', #10396, 1000.000000000000000 ) ;
#2543 = EDGE_CURVE ( 'NONE', #8501, #292, #5326, .T. ) ;
#2544 = ADVANCED_FACE ( 'NONE', ( #9424 ), #9366, .T. ) ;
#2545 = VERTEX_POINT ( 'NONE', #557 ) ;
#2546 = CYLINDRICAL_SURFACE ( 'NONE', #90, 3.000000000000000000 ) ;
#2547 = LINE ( 'NONE', #4182, #8651 ) ;
#2548 = PLANE ( 'NONE',  #5074 ) ;
#2549 = CARTESIAN_POINT ( 'NONE',  ( 10.69739119071655686, -10.02539999999999942, -12.00000000000000000 ) ) ;
#2550 = VECTOR ( 'NONE', #1462, 1000.000000000000000 ) ;
#2551 = CARTESIAN_POINT ( 'NONE',  ( 1.229367062500000163, -12.29022459553277002, -1.802083334016129967 ) ) ;
#2552 = CARTESIAN_POINT ( 'NONE',  ( 0.6479879772514793856, -4.687928535947285091, -0.01605171672202330979 ) ) ;
#2553 = ORIENTED_EDGE ( 'NONE', *, *, #203, .T. ) ;
#2554 = VECTOR ( 'NONE', #4552, 1000.000000000000000 ) ;
#2555 = DIRECTION ( 'NONE',  ( -1.156482317317871478E-16, 1.000000000000000000, 0.000000000000000000 ) ) ;
#2556 = CARTESIAN_POINT ( 'NONE',  ( 0.8603895577212593571, 5.432285873273261068, 2.519999999999999574 ) ) ;
#2557 = ADVANCED_FACE ( 'NONE', ( #6665 ), #9922, .F. ) ;
#2558 = CARTESIAN_POINT ( 'NONE',  ( 0.000000000000000000, -10.00000000000000000, 0.000000000000000000 ) ) ;
#2559 = AXIS2_PLACEMENT_3D ( 'NONE', #2037, #3619, #8558 ) ;
#2560 = CONTEXT_DEPENDENT_SHAPE_REPRESENTATION ( #8518, #6562 ) ;
#2561 = CARTESIAN_POINT ( 'NONE',  ( -0.8603895577212598011, -5.432285873273260179, 6.719999999999999751 ) ) ;
#2562 = APPLICATION_CONTEXT ( 'automotive_design' ) ;
#2563 = CARTESIAN_POINT ( 'NONE',  ( -2.000000000000000000, 8.357095590591340439, -1.552080310331536372 ) ) ;
#2564 = DIRECTION ( 'NONE',  ( -1.000000000000000000, -0.000000000000000000, -0.000000000000000000 ) ) ;
#2565 = CARTESIAN_POINT ( 'NONE',  ( -2.000000000000000000, 1.106368468154538931, -8.427689411260562480 ) ) ;
#2566 = CARTESIAN_POINT ( 'NONE',  ( -2.000000000000000000, -5.233522515400054864, -4.720195129223331065 ) ) ;
#2567 = CARTESIAN_POINT ( 'NONE',  ( -3.411736077305382420, 3.279728542977939476, 5.896051716722023883 ) ) ;
#2568 = SURFACE_STYLE_USAGE ( .BOTH. , #9034 ) ;
#2569 = CARTESIAN_POINT ( 'NONE',  ( 4.458484982038663169, 0.6162731882459350219, 7.683948283277975300 ) ) ;
#2570 = DIRECTION ( 'NONE',  ( 0.000000000000000000, 0.000000000000000000, 1.000000000000000000 ) ) ;
#2571 = ORIENTED_EDGE ( 'NONE', *, *, #671, .F. ) ;
#2572 = CARTESIAN_POINT ( 'NONE',  ( -5.110351332421769754, -2.708615832122969191, 5.336051716722022498 ) ) ;
#2573 = ORIENTED_EDGE ( 'NONE', *, *, #4410, .T. ) ;
#2574 = DIRECTION ( 'NONE',  ( 0.3420201433256627732, -0.9396926207859105373, 0.000000000000000000 ) ) ;
#2575 = LINE ( 'NONE', #5790, #7631 ) ;
#2576 = EDGE_LOOP ( 'NONE', ( #2888, #5204, #5800, #8674 ) ) ;
#2577 = CARTESIAN_POINT ( 'NONE',  ( -4.444597532678119300, -0.7039550926810477227, 4.479999999999999538 ) ) ;
#2578 = CARTESIAN_POINT ( 'NONE',  ( 0.000000000000000000, 0.000000000000000000, 5.999999999999999112 ) ) ;
#2579 = VERTEX_POINT ( 'NONE', #7015 ) ;
#2580 = CARTESIAN_POINT ( 'NONE',  ( -3.119207202478379681, -3.244753828200550139, 10.79605171672202246 ) ) ;
#2581 =( BOUNDED_CURVE ( )  B_SPLINE_CURVE ( 2, ( #4447, #279, #6935, #9182, #1972, #10089, #10193, #2709, #2862, #6886, #3504, #2074, #3554 ),
 .UNSPECIFIED., .F., .T. ) 
 B_SPLINE_CURVE_WITH_KNOTS ( ( 3, 2, 2, 2, 2, 2, 3 ),
 ( 0.8538060088535064374, 0.8611111111111111605, 0.8888888888888888395, 0.9166666666666666297, 0.9444444444444444198, 0.9722222222222222099, 1.000000000000000000 ),
 .UNSPECIFIED. ) 
 CURVE ( )  GEOMETRIC_REPRESENTATION_ITEM ( )  RATIONAL_B_SPLINE_CURVE ( ( 0.9480652127606681301, 0.9647668674900647945, 1.000000000000000000, 0.8660254037844387076, 1.000000000000000000, 0.8660254037844387076, 1.000000000000000000, 0.8660254037844387076, 1.000000000000000000, 0.8660254037844387076, 1.000000000000000000, 0.8660254037844387076, 1.000000000000000000 ) ) 
 REPRESENTATION_ITEM ( '' )  );
#2582 = FACE_OUTER_BOUND ( 'NONE', #708, .T. ) ;
#2583 = ORIENTED_EDGE ( 'NONE', *, *, #3437, .T. ) ;
#2584 =( LENGTH_UNIT ( ) NAMED_UNIT ( * ) SI_UNIT ( .MILLI., .METRE. ) );
#2585 = EDGE_LOOP ( 'NONE', ( #7497, #6215 ) ) ;
#2586 = EDGE_CURVE ( 'NONE', #3324, #3111, #456, .T. ) ;
#2587 = LINE ( 'NONE', #4912, #5994 ) ;
#2588 = DIRECTION ( 'NONE',  ( -1.000000000000000000, -0.000000000000000000, -0.000000000000000000 ) ) ;
#2589 = VERTEX_POINT ( 'NONE', #3684 ) ;
#2590 = CARTESIAN_POINT ( 'NONE',  ( -5.711843387010018702, 0.9046671180729746187, 1.819999999999999396 ) ) ;
#2591 = ADVANCED_BREP_SHAPE_REPRESENTATION ( '', ( #7952, #2101 ), #8215 ) ;
#2592 = CARTESIAN_POINT ( 'NONE',  ( 5.432285873273257515, 0.8603895577212793411, 0.2799999999999999156 ) ) ;
#2593 = CARTESIAN_POINT ( 'NONE',  ( -0.8124729078102072011, 5.726445515403652209, 9.783948283277975833 ) ) ;
#2594 = ORIENTED_EDGE ( 'NONE', *, *, #5708, .T. ) ;
#2595 = CARTESIAN_POINT ( 'NONE',  ( 8.692241771943169307E-17, -11.58044919106553294, -1.093750000682796486 ) ) ;
#2596 = ADVANCED_FACE ( 'NONE', ( #8570 ), #2893, .T. ) ;
#2597 = VECTOR ( 'NONE', #4595, 1000.000000000000000 ) ;
#2598 = EDGE_LOOP ( 'NONE', ( #5762, #1261, #3804, #1806 ) ) ;
#2599 = DIRECTION ( 'NONE',  ( -1.000000000000000000, 0.000000000000000000, -0.000000000000000000 ) ) ;
#2600 = CARTESIAN_POINT ( 'NONE',  ( 6.727620669667255804, -7.750000000000000000, 0.000000000000000000 ) ) ;
#2601 = DIRECTION ( 'NONE',  ( 0.3420201433256627732, -0.9396926207859105373, 0.000000000000000000 ) ) ;
#2602 = ORIENTED_EDGE ( 'NONE', *, *, #4777, .F. ) ;
#2603 = DIRECTION ( 'NONE',  ( 0.000000000000000000, 0.000000000000000000, 1.000000000000000000 ) ) ;
#2604 = VECTOR ( 'NONE', #8009, 1000.000000000000000 ) ;
#2605 = CARTESIAN_POINT ( 'NONE',  ( 0.6146835312499993043, -14.06466310670085562, -1.927083334016129967 ) ) ;
#2606 = CARTESIAN_POINT ( 'NONE',  ( -3.244753828200538148, -3.119207202478392116, 0.4039482832779765498 ) ) ;
#2607 = EDGE_CURVE ( 'NONE', #9521, #8600, #1543, .T. ) ;
#2608 = VERTEX_POINT ( 'NONE', #660 ) ;
#2609 = EDGE_CURVE ( 'NONE', #1584, #4442, #1573, .T. ) ;
#2610 = CARTESIAN_POINT ( 'NONE',  ( 25.00000000000000000, -4.000000000000000000, -2.000000000000000000 ) ) ;
#2611 = CARTESIAN_POINT ( 'NONE',  ( -4.089228379062038066, 4.089228379062021190, 2.099999999999999201 ) ) ;
#2612 = CARTESIAN_POINT ( 'NONE',  ( 0.000000000000000000, -13.00000000000000533, 0.000000000000000000 ) ) ;
#2613 = CARTESIAN_POINT ( 'NONE',  ( -3.889087296526005044, -3.889087296526019255, 6.999999999999999112 ) ) ;
#2614 = CYLINDRICAL_SURFACE ( 'NONE', #7378, 3.000000000000000000 ) ;
#2615 = FACE_OUTER_BOUND ( 'NONE', #4464, .T. ) ;
#2616 = DIRECTION ( 'NONE',  ( 0.000000000000000000, 1.000000000000000000, -7.228014483236698281E-18 ) ) ;
#2617 = CARTESIAN_POINT ( 'NONE',  ( 3.411736077305382420, -3.279728542977940364, 1.696051716722023484 ) ) ;
#2618 = EDGE_CURVE ( 'NONE', #9748, #6164, #2363, .T. ) ;
#2619 = CARTESIAN_POINT ( 'NONE',  ( -1.229367062500000163, -13.00000000000000533, -2.468750000682796486 ) ) ;
#2620 = VECTOR ( 'NONE', #1316, 1000.000000000000000 ) ;
#2621 = CARTESIAN_POINT ( 'NONE',  ( 1.963858260114715870, -4.049832306626327316, 2.643948283277976596 ) ) ;
#2622 = DIRECTION ( 'NONE',  ( 0.000000000000000000, 0.000000000000000000, 1.000000000000000000 ) ) ;
#2623 = ORIENTED_EDGE ( 'NONE', *, *, #2428, .T. ) ;
#2624 = CARTESIAN_POINT ( 'NONE',  ( -0.9968613283357868893, 5.697241258616382531, 3.376051716722022977 ) ) ;
#2625 = DIRECTION ( 'NONE',  ( 0.000000000000000000, 0.000000000000000000, 1.000000000000000000 ) ) ;
#2626 = PLANE ( 'NONE',  #1712 ) ;
#2627 = EDGE_LOOP ( 'NONE', ( #6418, #4531, #6663, #339 ) ) ;
#2628 = EDGE_CURVE ( 'NONE', #3378, #9951, #7179, .T. ) ;
#2629 = DIRECTION ( 'NONE',  ( -0.000000000000000000, -0.000000000000000000, -1.000000000000000000 ) ) ;
#2630 = ORIENTED_EDGE ( 'NONE', *, *, #9628, .F. ) ;
#2631 = CARTESIAN_POINT ( 'NONE',  ( 4.173491630687861331, 2.231261971483781359, 12.33605171672202339 ) ) ;
#2632 = CARTESIAN_POINT ( 'NONE',  ( 8.692241771943169307E-17, -11.58044919106553294, -2.718750000682796042 ) ) ;
#2633 = VERTEX_POINT ( 'NONE', #1403 ) ;
#2634 = DIRECTION ( 'NONE',  ( 0.000000000000000000, 1.156482317317871478E-16, -1.000000000000000000 ) ) ;
#2635 = AXIS2_PLACEMENT_3D ( 'NONE', #6766, #10075, #2164 ) ;
#2636 = VERTEX_POINT ( 'NONE', #8833 ) ;
#2637 = LINE ( 'NONE', #5750, #7200 ) ;
#2638 = CARTESIAN_POINT ( 'NONE',  ( 1.530808498934183189E-16, -27.00000000000000711, 1.249999999999993339 ) ) ;
#2639 = ORIENTED_EDGE ( 'NONE', *, *, #5366, .T. ) ;
#2640 = CARTESIAN_POINT ( 'NONE',  ( 5.711843387010018702, -0.9046671180729751738, 11.61999999999999922 ) ) ;
#2641 = ADVANCED_FACE ( 'NONE', ( #3893 ), #9530, .T. ) ;
#2642 = CARTESIAN_POINT ( 'NONE',  ( -5.711843387010018702, 0.9046671180729746187, 7.419999999999998153 ) ) ;
#2643 = CARTESIAN_POINT ( 'NONE',  ( -2.496947748567517333, 4.900535883036019058, 7.839999999999999858 ) ) ;
#2644 = VERTEX_POINT ( 'NONE', #3208 ) ;
#2645 = AXIS2_PLACEMENT_3D ( 'NONE', #4504, #3814, #2819 ) ;
#2646 = CARTESIAN_POINT ( 'NONE',  ( -1.229367062500000385, -13.70977540446723886, -0.4270833340161298564 ) ) ;
#2647 = VECTOR ( 'NONE', #3350, 1000.000000000000000 ) ;
#2648 = ORIENTED_EDGE ( 'NONE', *, *, #6651, .F. ) ;
#2649 = CARTESIAN_POINT ( 'NONE',  ( 10.00000000000000000, 7.003298780661491918, -4.817032923780498521 ) ) ;
#2650 = EDGE_CURVE ( 'NONE', #5636, #525, #5431, .T. ) ;
#2651 = DIRECTION ( 'NONE',  ( -1.000000000000000000, 0.000000000000000000, -0.000000000000000000 ) ) ;
#2652 = DIRECTION ( 'NONE',  ( -5.694029147589358720E-15, -6.585044023479645679E-31, 1.000000000000000000 ) ) ;
#2653 = VERTEX_POINT ( 'NONE', #4740 ) ;
#2654 = CARTESIAN_POINT ( 'NONE',  ( 30.00000000000001066, 0.000000000000000000, 0.000000000000000000 ) ) ;
#2655 = CARTESIAN_POINT ( 'NONE',  ( 1.229367062500000163, -13.00000000000000533, -1.843750000682796708 ) ) ;
#2656 = CARTESIAN_POINT ( 'NONE',  ( -2.231261971483764484, -4.173491630687871101, 0.2639482832779765920 ) ) ;
#2657 = ORIENTED_EDGE ( 'NONE', *, *, #5102, .T. ) ;
#2658 = DIRECTION ( 'NONE',  ( 0.000000000000000000, 0.000000000000000000, 1.000000000000000000 ) ) ;
#2659 = CARTESIAN_POINT ( 'NONE',  ( -3.889087296526005044, -3.889087296526019255, 12.59999999999999787 ) ) ;
#2660 = DIRECTION ( 'NONE',  ( 0.000000000000000000, -0.000000000000000000, 1.000000000000000000 ) ) ;
#2661 = CARTESIAN_POINT ( 'NONE',  ( 5.711843387010019590, -0.9046671180729753958, 11.61999999999999922 ) ) ;
#2662 = EDGE_CURVE ( 'NONE', #10188, #2753, #3156, .T. ) ;
#2663 = CARTESIAN_POINT ( 'NONE',  ( -26.99999999999998579, -32.00000000000000000, 9.000000000000000000 ) ) ;
#2664 = DIRECTION ( 'NONE',  ( -1.000000000000000000, -0.000000000000000000, 0.000000000000000000 ) ) ;
#2665 = DIRECTION ( 'NONE',  ( 0.000000000000000000, 0.000000000000000000, -1.000000000000000000 ) ) ;
#2666 = CARTESIAN_POINT ( 'NONE',  ( 2.122056237541221524, -3.969226411068978777, 1.836051716722023386 ) ) ;
#2667 = CARTESIAN_POINT ( 'NONE',  ( 0.6146835312499993043, -14.06466310670085562, -1.302083334016129967 ) ) ;
#2668 = CARTESIAN_POINT ( 'NONE',  ( -4.658724279160018078, 0.8323763977770419764, 3.623948283277976135 ) ) ;
#2669 = CARTESIAN_POINT ( 'NONE',  ( 10.00000000000000000, 7.008469740302810891, -0.7425307242147085596 ) ) ;
#2670 = VERTEX_POINT ( 'NONE', #6216 ) ;
#2671 = EDGE_CURVE ( 'NONE', #7286, #7942, #9636, .T. ) ;
#2672 = CARTESIAN_POINT ( 'NONE',  ( -2.542276634908081423, -5.195105386651227342, 2.256051716722022871 ) ) ;
#2673 = EDGE_CURVE ( 'NONE', #376, #8882, #4052, .T. ) ;
#2674 = DIRECTION ( 'NONE',  ( 0.000000000000000000, 8.881784197001252323E-16, -1.000000000000000000 ) ) ;
#2675 = DIRECTION ( 'NONE',  ( 0.3420201433256627732, -0.9396926207859105373, 0.000000000000000000 ) ) ;
#2676 = ORIENTED_EDGE ( 'NONE', *, *, #9614, .T. ) ;
#2677 = CARTESIAN_POINT ( 'NONE',  ( 0.7401821875142697849, -4.673326407553650697, 12.17999999999999616 ) ) ;
#2678 = EDGE_CURVE ( 'NONE', #1372, #274, #2849, .T. ) ;
#2679 = CARTESIAN_POINT ( 'NONE',  ( -2.064922774268895811, -4.258245684917318918, 5.056051716722023137 ) ) ;
#2680 = FACE_OUTER_BOUND ( 'NONE', #7404, .T. ) ;
#2681 = ORIENTED_EDGE ( 'NONE', *, *, #9656, .F. ) ;
#2682 = EDGE_CURVE ( 'NONE', #3139, #3971, #362, .T. ) ;
#2683 = DIRECTION ( 'NONE',  ( 1.000000000000000000, 0.000000000000000000, 0.000000000000000000 ) ) ;
#2684 = ORIENTED_EDGE ( 'NONE', *, *, #6082, .F. ) ;
#2685 = DIRECTION ( 'NONE',  ( 1.000000000000000000, -0.000000000000000000, -0.000000000000000000 ) ) ;
#2686 = CARTESIAN_POINT ( 'NONE',  ( 23.86937280323380506, -10.00000000000000178, 0.000000000000000000 ) ) ;
#2687 = ORIENTED_EDGE ( 'NONE', *, *, #5598, .T. ) ;
#2688 = CARTESIAN_POINT ( 'NONE',  ( 5.110351332421769754, 2.708615832122969191, 1.136051716722023208 ) ) ;
#2689 = CARTESIAN_POINT ( 'NONE',  ( -2.496947748567517333, 4.900535883036019058, 2.239999999999999769 ) ) ;
#2690 = CARTESIAN_POINT ( 'NONE',  ( -5.432285873273256627, -0.8603895577212797852, 12.87999999999999901 ) ) ;
#2691 = ORIENTED_EDGE ( 'NONE', *, *, #8760, .F. ) ;
#2692 = CARTESIAN_POINT ( 'NONE',  ( -0.6146835312499998594, -11.93533689329915326, -2.052083334016129967 ) ) ;
#2693 = VECTOR ( 'NONE', #5458, 1000.000000000000000 ) ;
#2694 = EDGE_LOOP ( 'NONE', ( #8630, #5482, #9256, #6327 ) ) ;
#2695 = CARTESIAN_POINT ( 'NONE',  ( 25.00000000000000000, 0.000000000000000000, -10.00000000000000000 ) ) ;
#2696 = VECTOR ( 'NONE', #2754, 1000.000000000000000 ) ;
#2697 = CARTESIAN_POINT ( 'NONE',  ( 15.00000000000000000, 19.99999999999999645, -9.000000000000000000 ) ) ;
#2698 = ORIENTED_EDGE ( 'NONE', *, *, #150, .F. ) ;
#2699 = CARTESIAN_POINT ( 'NONE',  ( 1.530808498934180724E-16, 26.99999999999999289, -1.249999999999988898 ) ) ;
#2700 = AXIS2_PLACEMENT_3D ( 'NONE', #3352, #3198, #6422 ) ;
#2701 = CARTESIAN_POINT ( 'NONE',  ( 1.229367062500000163, -12.29022459553277002, -2.302083334016129967 ) ) ;
#2702 = CARTESIAN_POINT ( 'NONE',  ( -0.6479879772514802738, 4.687928535947285091, 12.58394828327797477 ) ) ;
#2703 = ORIENTED_EDGE ( 'NONE', *, *, #4097, .F. ) ;
#2704 = VECTOR ( 'NONE', #1155, 1000.000000000000000 ) ;
#2705 = DIRECTION ( 'NONE',  ( 0.000000000000000000, 0.000000000000000000, 1.000000000000000000 ) ) ;
#2706 = VECTOR ( 'NONE', #1732, 1000.000000000000000 ) ;
#2707 = CARTESIAN_POINT ( 'NONE',  ( 0.9046671180729951578, -5.711843387010016926, 9.379999999999995453 ) ) ;
#2708 = EDGE_CURVE ( 'NONE', #5056, #1737, #6433, .T. ) ;
#2709 = CARTESIAN_POINT ( 'NONE',  ( -1.500000000000000666, -13.86602540378444637, 0.2291666653010732135 ) ) ;
#2710 = CARTESIAN_POINT ( 'NONE',  ( 4.089228379062037178, -4.089228379062022967, 11.89999999999999858 ) ) ;
#2711 = VECTOR ( 'NONE', #2588, 1000.000000000000000 ) ;
#2712 = DIRECTION ( 'NONE',  ( -0.000000000000000000, 0.8660254037844391517, 0.4999999999999991118 ) ) ;
#2713 = CIRCLE ( 'NONE', #9322, 6.248999999999999666 ) ;
#2714 = DIRECTION ( 'NONE',  ( -1.000000000000000000, 0.000000000000000000, 0.000000000000000000 ) ) ;
#2715 = DIRECTION ( 'NONE',  ( 0.000000000000000000, 0.000000000000000000, 1.000000000000000000 ) ) ;
#2716 = CARTESIAN_POINT ( 'NONE',  ( -0.7039550926810301812, -4.444597532678121965, 1.119999999999999885 ) ) ;
#2717 = DIRECTION ( 'NONE',  ( 1.000000000000000000, 0.000000000000000000, 0.000000000000000000 ) ) ;
#2718 = EDGE_CURVE ( 'NONE', #8842, #1757, #7122, .T. ) ;
#2719 = CARTESIAN_POINT ( 'NONE',  ( -1.963858260114716980, 4.049832306626327316, 12.44394828327797597 ) ) ;
#2720 = VECTOR ( 'NONE', #5313, 1000.000000000000000 ) ;
#2721 = CARTESIAN_POINT ( 'NONE',  ( 22.43558391966725907, -7.750000000000000000, 0.000000000000000000 ) ) ;
#2723 = ORIENTED_EDGE ( 'NONE', *, *, #6351, .T. ) ;
#2722 = AXIS2_PLACEMENT_3D ( 'NONE', #3461, #5099, #7702 ) ;
#2724 = CARTESIAN_POINT ( 'NONE',  ( -5.418398423912711870, -0.9480714621563917088, 8.276051716722021112 ) ) ;
#2725 = VECTOR ( 'NONE', #4629, 1000.000000000000000 ) ;
#2726 = CARTESIAN_POINT ( 'NONE',  ( 0.000000000000000000, -10.00000000000000000, 0.000000000000000000 ) ) ;
#2727 = CIRCLE ( 'NONE', #10351, 3.000000000000000888 ) ;
#2728 = DIRECTION ( 'NONE',  ( 0.000000000000000000, 0.000000000000000000, -1.000000000000000000 ) ) ;
#2729 = VERTEX_POINT ( 'NONE', #719 ) ;
#2730 = CARTESIAN_POINT ( 'NONE',  ( 4.009529358847659708, -2.042957248827953709, 11.75999999999999979 ) ) ;
#2731 = AXIS2_PLACEMENT_3D ( 'NONE', #725, #5540, #10443 ) ;
#2732 =( NAMED_UNIT ( * ) PLANE_ANGLE_UNIT ( ) SI_UNIT ( $, .RADIAN. ) );
#2733 = EDGE_CURVE ( 'NONE', #7510, #1757, #6609, .T. ) ;
#2734 = EDGE_CURVE ( 'NONE', #145, #1958, #7815, .T. ) ;
#2735 = CARTESIAN_POINT ( 'NONE',  ( 2.148092372876330369, 4.215868657802593233, 2.659999999999998366 ) ) ;
#2736 = VECTOR ( 'NONE', #8300, 1000.000000000000000 ) ;
#2737 = CARTESIAN_POINT ( 'NONE',  ( -0.6146835312500006365, -14.06466310670085562, -2.510416667349463005 ) ) ;
#2738 = VERTEX_POINT ( 'NONE', #4684 ) ;
#2739 = DIRECTION ( 'NONE',  ( 5.669560381884707106E-30, -1.000000000000000222, -8.789265611615816038E-17 ) ) ;
#2740 = ORIENTED_EDGE ( 'NONE', *, *, #3234, .F. ) ;
#2741 = CARTESIAN_POINT ( 'NONE',  ( 0.7499999999999991118, -14.29903810567666333, -0.5833333333333332593 ) ) ;
#2742 = CARTESIAN_POINT ( 'NONE',  ( 25.00000000000000000, 3.750000000000000000, -12.00000000000000000 ) ) ;
#2743 = ORIENTED_EDGE ( 'NONE', *, *, #3577, .T. ) ;
#2744 = CARTESIAN_POINT ( 'NONE',  ( 0.9968613283357860011, -5.697241258616382531, 4.776051716722021112 ) ) ;
#2745 = CARTESIAN_POINT ( 'NONE',  ( 5.152728359536493663, 2.625446233515533745, 2.939999999999999059 ) ) ;
#2746 = CARTESIAN_POINT ( 'NONE',  ( -2.625446233515515981, -5.152728359536500768, 6.859999999999999432 ) ) ;
#2747 = ORIENTED_EDGE ( 'NONE', *, *, #2816, .T. ) ;
#2748 = EDGE_CURVE ( 'NONE', #5539, #4283, #9339, .T. ) ;
#2749 = CARTESIAN_POINT ( 'NONE',  ( -1.229367062500000163, -12.29022459553277002, -2.010416667349463005 ) ) ;
#2750 = ORIENTED_EDGE ( 'NONE', *, *, #9279, .F. ) ;
#2751 = DIRECTION ( 'NONE',  ( 0.000000000000000000, 0.000000000000000000, -1.000000000000000000 ) ) ;
#2752 = CARTESIAN_POINT ( 'NONE',  ( 8.161409553233804459, 6.000000000000000000, -12.00000000000000000 ) ) ;
#2753 = VERTEX_POINT ( 'NONE', #3103 ) ;
#2754 = DIRECTION ( 'NONE',  ( 1.000000000000000000, -0.000000000000000000, -0.000000000000000000 ) ) ;
#2755 = LINE ( 'NONE', #8923, #10185 ) ;
#2756 = CARTESIAN_POINT ( 'NONE',  ( 1.229367062500000163, -13.70977540446723886, -1.885416667349463449 ) ) ;
#2757 = CARTESIAN_POINT ( 'NONE',  ( 3.951860609387084722, 3.826313983664940022, -0.9960517167220231949 ) ) ;
#2758 = ORIENTED_EDGE ( 'NONE', *, *, #9103, .F. ) ;
#2759 = EDGE_CURVE ( 'NONE', #1744, #618, #8091, .T. ) ;
#2760 = FACE_OUTER_BOUND ( 'NONE', #8587, .T. ) ;
#2761 = CARTESIAN_POINT ( 'NONE',  ( -5.432285873273256627, -0.8603895577212797852, 10.07999999999999829 ) ) ;
#2762 = DIRECTION ( 'NONE',  ( -1.000000000000000000, -0.000000000000000000, 0.000000000000000000 ) ) ;
#2763 = CARTESIAN_POINT ( 'NONE',  ( 2.496947748567516889, -4.900535883036019946, 6.439999999999999503 ) ) ;
#2764 = VECTOR ( 'NONE', #1540, 1000.000000000000000 ) ;
#2765 = DIRECTION ( 'NONE',  ( 0.000000000000000000, 0.000000000000000000, 1.000000000000000000 ) ) ;
#2766 = CARTESIAN_POINT ( 'NONE',  ( 27.00000000000001066, -25.00000000000000000, 0.000000000000000000 ) ) ;
#2767 = ADVANCED_FACE ( 'NONE', ( #8252 ), #8931, .F. ) ;
#2768 = DIRECTION ( 'NONE',  ( 0.000000000000000000, -1.000000000000000000, 0.000000000000000000 ) ) ;
#2769 = CARTESIAN_POINT ( 'NONE',  ( -3.181980515339458027, -3.181980515339470905, 1.399999999999999689 ) ) ;
#2770 = CARTESIAN_POINT ( 'NONE',  ( 1.229367062500000163, -13.00000000000000533, -2.218750000682796486 ) ) ;
#2771 = CARTESIAN_POINT ( 'NONE',  ( 4.658724279160018966, -0.8323763977770426425, 10.62394828327797569 ) ) ;
#2772 = ADVANCED_FACE ( 'NONE', ( #4255 ), #9847, .F. ) ;
#2773 = CARTESIAN_POINT ( 'NONE',  ( -0.6146835312499998594, -11.93533689329915326, -0.05208333401612993963 ) ) ;
#2774 = ORIENTED_EDGE ( 'NONE', *, *, #8236, .T. ) ;
#2775 = CARTESIAN_POINT ( 'NONE',  ( -4.155232146225753098, 4.023224611898306158, 3.096051716722023617 ) ) ;
#2776 = DIRECTION ( 'NONE',  ( 1.000000000000000000, 0.000000000000000000, 0.000000000000000000 ) ) ;
#2777 = ADVANCED_FACE ( 'NONE', ( #5789 ), #6540, .F. ) ;
#2778 = DIRECTION ( 'NONE',  ( 1.000000000000000000, 0.000000000000000000, 0.000000000000000000 ) ) ;
#2779 = ORIENTED_EDGE ( 'NONE', *, *, #6684, .F. ) ;
#2780 = AXIS2_PLACEMENT_3D ( 'NONE', #5396, #4602, #8692 ) ;
#2781 = CARTESIAN_POINT ( 'NONE',  ( 0.7401821875142697849, -4.673326407553650697, 9.379999999999997229 ) ) ;
#2782 =( LENGTH_UNIT ( ) NAMED_UNIT ( * ) SI_UNIT ( .MILLI., .METRE. ) );
#2783 = CARTESIAN_POINT ( 'NONE',  ( 2.148092372876330369, 4.215868657802593233, 5.459999999999997300 ) ) ;
#2784 = CARTESIAN_POINT ( 'NONE',  ( -2.607672531582950546E-16, -14.41955080893447416, -0.9687500006827967081 ) ) ;
#2785 = EDGE_LOOP ( 'NONE', ( #9422, #9659, #2187, #3100 ) ) ;
#2786 = DIRECTION ( 'NONE',  ( 1.000000000000000000, 0.000000000000000000, 0.000000000000000000 ) ) ;
#2787 = ORIENTED_EDGE ( 'NONE', *, *, #3451, .F. ) ;
#2788 = CARTESIAN_POINT ( 'NONE',  ( -3.181725716174720991E-16, -14.73205080756888563, -0.6250000000000001110 ) ) ;
#2789 = DIRECTION ( 'NONE',  ( 0.000000000000000000, 0.000000000000000000, 1.000000000000000000 ) ) ;
#2790 = ORIENTED_EDGE ( 'NONE', *, *, #5642, .F. ) ;
#2791 = CARTESIAN_POINT ( 'NONE',  ( 3.826313983664925811, 3.951860609387098044, 0.9960517167220231949 ) ) ;
#2792 = EDGE_CURVE ( 'NONE', #5123, #2426, #7305, .T. ) ;
#2793 = CARTESIAN_POINT ( 'NONE',  ( -2.496947748567517333, 4.900535883036019058, 10.63999999999999879 ) ) ;
#2794 = STYLED_ITEM ( 'NONE', ( #8362 ), #9161 ) ;
#2795 = CARTESIAN_POINT ( 'NONE',  ( 0.9046671180729951578, -5.711843387010016926, 12.17999999999999439 ) ) ;
#2796 = VERTEX_POINT ( 'NONE', #1779 ) ;
#2797 = CARTESIAN_POINT ( 'NONE',  ( 1.300000000000000044, 1.478016689125442484, -1.626303258728256651E-15 ) ) ;
#2798 = CIRCLE ( 'NONE', #1623, 2.000000000000001776 ) ;
#2799 = DIRECTION ( 'NONE',  ( 0.000000000000000000, 0.000000000000000000, 1.000000000000000000 ) ) ;
#2800 = ORIENTED_EDGE ( 'NONE', *, *, #2416, .F. ) ;
#2801 = EDGE_CURVE ( 'NONE', #4853, #8842, #7343, .T. ) ;
#2802 = FACE_OUTER_BOUND ( 'NONE', #9843, .T. ) ;
#2803 = EDGE_CURVE ( 'NONE', #3690, #48, #6692, .T. ) ;
#2804 = DIRECTION ( 'NONE',  ( -5.637851296924623057E-15, -6.520075332560955295E-31, 1.000000000000000000 ) ) ;
#2805 = ORIENTED_EDGE ( 'NONE', *, *, #6723, .T. ) ;
#2806 = FACE_OUTER_BOUND ( 'NONE', #2320, .T. ) ;
#2807 = VECTOR ( 'NONE', #6939, 1000.000000000000000 ) ;
#2808 = DIRECTION ( 'NONE',  ( 0.000000000000000000, 2.486899575160350966E-14, -1.000000000000000000 ) ) ;
#2809 = DIRECTION ( 'NONE',  ( 1.000000000000000000, 0.000000000000000000, 0.000000000000000000 ) ) ;
#2810 = CARTESIAN_POINT ( 'NONE',  ( 2.417848759854264618, -4.940838830814695548, -0.1560517167220233370 ) ) ;
#2811 = ORIENTED_EDGE ( 'NONE', *, *, #9703, .F. ) ;
#2812 = AXIS2_PLACEMENT_3D ( 'NONE', #9834, #2564, #5778 ) ;
#2813 = DIRECTION ( 'NONE',  ( 1.000000000000000000, 0.000000000000000000, 0.000000000000000000 ) ) ;
#2814 = CARTESIAN_POINT ( 'NONE',  ( 3.889087296526005488, 3.889087296526018811, 11.19999999999999751 ) ) ;
#2815 = LINE ( 'NONE', #6781, #5977 ) ;
#2816 = EDGE_CURVE ( 'NONE', #4169, #6012, #5735, .T. ) ;
#2817 = CARTESIAN_POINT ( 'NONE',  ( 0.7499999999999991118, -14.29903810567666333, -0.08333333333333370341 ) ) ;
#2818 = AXIS2_PLACEMENT_3D ( 'NONE', #6404, #8911, #6513 ) ;
#2819 = DIRECTION ( 'NONE',  ( 1.000000000000000000, 0.000000000000000000, 0.000000000000000000 ) ) ;
#2820 = DIRECTION ( 'NONE',  ( 0.000000000000000000, 0.000000000000000000, 1.000000000000000000 ) ) ;
#2821 = CARTESIAN_POINT ( 'NONE',  ( -4.000000000000000000, -13.00000000000000533, 2.000000000000000000 ) ) ;
#2822 = CARTESIAN_POINT ( 'NONE',  ( 4.049832306626335310, -1.963858260114701215, 12.75605171672202331 ) ) ;
#2823 = CARTESIAN_POINT ( 'NONE',  ( 0.6146835312500001924, -11.93533689329915326, -1.635416667349463227 ) ) ;
#2824 = CARTESIAN_POINT ( 'NONE',  ( 3.951860609387084722, 3.826313983664940022, 1.803948283277976516 ) ) ;
#2825 = CARTESIAN_POINT ( 'NONE',  ( -1.229367062500000163, -12.29022459553277002, -0.01041666734946308792 ) ) ;
#2826 = ORIENTED_EDGE ( 'NONE', *, *, #2998, .F. ) ;
#2827 = FACE_OUTER_BOUND ( 'NONE', #1857, .T. ) ;
#2828 = AXIS2_PLACEMENT_3D ( 'NONE', #5097, #9941, #2665 ) ;
#2829 = LINE ( 'NONE', #393, #4246 ) ;
#2830 = DIRECTION ( 'NONE',  ( 0.3420201433256627732, 0.9396926207859105373, 0.000000000000000000 ) ) ;
#2831 = ORIENTED_EDGE ( 'NONE', *, *, #7501, .F. ) ;
#2832 = CARTESIAN_POINT ( 'NONE',  ( 4.215868657802586128, 2.148092372876346801, 8.539999999999999147 ) ) ;
#2833 = CARTESIAN_POINT ( 'NONE',  ( -4.444597532678119300, -0.7039550926810477227, 4.479999999999999538 ) ) ;
#2834 = CARTESIAN_POINT ( 'NONE',  ( 0.6146835312500001924, -11.93533689329915326, -1.260416667349463227 ) ) ;
#2835 = VERTEX_POINT ( 'NONE', #3312 ) ;
#2836 = DIRECTION ( 'NONE',  ( 0.000000000000000000, -7.847870334214135379E-05, 0.9999999969205466410 ) ) ;
#2837 = ORIENTED_EDGE ( 'NONE', *, *, #9217, .F. ) ;
#2838 = CARTESIAN_POINT ( 'NONE',  ( -1.500000000000000222, -13.00000000000000533, -0.7500000000000002220 ) ) ;
#2839 = LINE ( 'NONE', #1999, #5763 ) ;
#2840 = CARTESIAN_POINT ( 'NONE',  ( -15.00000000000000000, 19.99999999999999645, 6.000000000000000000 ) ) ;
#2841 = EDGE_LOOP ( 'NONE', ( #560, #5127 ) ) ;
#2842 = CARTESIAN_POINT ( 'NONE',  ( -4.900535883036028828, 2.496947748567499126, 13.15999999999999837 ) ) ;
#2843 = CARTESIAN_POINT ( 'NONE',  ( -4.089228379062038066, 4.089228379062021190, 13.29999999999999538 ) ) ;
#2844 = CARTESIAN_POINT ( 'NONE',  ( -2.625446233515515981, -5.152728359536500768, 9.659999999999994813 ) ) ;
#2845 = EDGE_LOOP ( 'NONE', ( #5155, #8158, #55, #3121 ) ) ;
#2846 = FACE_OUTER_BOUND ( 'NONE', #33, .T. ) ;
#2847 = EDGE_CURVE ( 'NONE', #9902, #7878, #4204, .T. ) ;
#2848 = ORIENTED_EDGE ( 'NONE', *, *, #10393, .T. ) ;
#2849 =( BOUNDED_CURVE ( )  B_SPLINE_CURVE ( 2, ( #5585, #2311, #7875, #5481, #5534, #7988, #4007 ),
 .UNSPECIFIED., .F., .F. ) 
 B_SPLINE_CURVE_WITH_KNOTS ( ( 3, 2, 2, 3 ),
 ( 0.6666666666666666297, 0.6944444444444444198, 0.7222222222222222099, 0.7500000000000000000 ),
 .UNSPECIFIED. ) 
 CURVE ( )  GEOMETRIC_REPRESENTATION_ITEM ( )  RATIONAL_B_SPLINE_CURVE ( ( 1.000000000000000000, 0.8660254037844387076, 1.000000000000000000, 0.8660254037844387076, 1.000000000000000000, 0.8660254037844387076, 1.000000000000000000 ) ) 
 REPRESENTATION_ITEM ( '' )  );
#2850 = LINE ( 'NONE', #5182, #4651 ) ;
#2851 = CARTESIAN_POINT ( 'NONE',  ( 0.000000000000000000, 18.99999999999999289, 0.000000000000000000 ) ) ;
#2852 = ORIENTED_EDGE ( 'NONE', *, *, #2650, .T. ) ;
#2853 = DIRECTION ( 'NONE',  ( -1.000000000000000000, 0.000000000000000000, -0.000000000000000000 ) ) ;
#2854 = DIRECTION ( 'NONE',  ( 0.000000000000000000, -1.598721155460225418E-14, -1.000000000000000000 ) ) ;
#2855 = DIRECTION ( 'NONE',  ( 1.000000000000000000, 0.000000000000000000, 0.000000000000000000 ) ) ;
#2856 = CARTESIAN_POINT ( 'NONE',  ( -1.963858260114716980, 4.049832306626327316, 12.44394828327797597 ) ) ;
#2857 = ORIENTED_EDGE ( 'NONE', *, *, #1982, .F. ) ;
#2858 = CARTESIAN_POINT ( 'NONE',  ( -1.500000000000000666, -13.86602540378444459, -2.270833334698926453 ) ) ;
#2859 = EDGE_CURVE ( 'NONE', #789, #2419, #6641, .T. ) ;
#2860 = EDGE_CURVE ( 'NONE', #8371, #6113, #4584, .T. ) ;
#2861 = CARTESIAN_POINT ( 'NONE',  ( 3.889087296526005488, 3.889087296526018811, 13.99999999999999822 ) ) ;
#2862 = CARTESIAN_POINT ( 'NONE',  ( -0.7500000000000007772, -14.29903810567666156, 0.2708333319677396211 ) ) ;
#2863 = DIRECTION ( 'NONE',  ( 0.3420201433256627732, 0.9396926207859105373, -0.000000000000000000 ) ) ;
#2864 = CARTESIAN_POINT ( 'NONE',  ( 0.1499999999999973577, 0.000000000000000000, 0.000000000000000000 ) ) ;
#2865 = CARTESIAN_POINT ( 'NONE',  ( 6.727620669667255804, 3.750000000000000000, 0.000000000000000000 ) ) ;
#2866 = AXIS2_PLACEMENT_3D ( 'NONE', #981, #8934, #10494 ) ;
#2867 = CYLINDRICAL_SURFACE ( 'NONE', #4713, 3.000000000000000000 ) ;
#2868 = CARTESIAN_POINT ( 'NONE',  ( -3.119207202478379681, -3.244753828200550139, 13.59605171672202140 ) ) ;
#2869 = VECTOR ( 'NONE', #7032, 1000.000000000000000 ) ;
#2870 = CARTESIAN_POINT ( 'NONE',  ( -1.229367062500000385, -13.70977540446723886, -2.052083334016129967 ) ) ;
#2871 = EDGE_CURVE ( 'NONE', #2310, #2589, #6449, .T. ) ;
#2872 = CARTESIAN_POINT ( 'NONE',  ( -4.023224611898323033, 4.155232146225737111, 3.903948283277975939 ) ) ;
#2873 = CARTESIAN_POINT ( 'NONE',  ( 1.229367062500000163, -12.29022459553277002, -1.677083334016129967 ) ) ;
#2874 = ORIENTED_EDGE ( 'NONE', *, *, #9103, .T. ) ;
#2875 = VECTOR ( 'NONE', #6047, 1000.000000000000000 ) ;
#2876 = CARTESIAN_POINT ( 'NONE',  ( 5.999999999999999112, -27.00000000000000711, 3.000000000000000000 ) ) ;
#2877 = EDGE_CURVE ( 'NONE', #9435, #1470, #9790, .T. ) ;
#2878 = DIRECTION ( 'NONE',  ( -1.000000000000000000, 0.000000000000000000, -0.000000000000000000 ) ) ;
#2879 = LINE ( 'NONE', #9194, #5845 ) ;
#2880 = CARTESIAN_POINT ( 'NONE',  ( 10.00000000000000000, -8.497168642645963388, -0.2193742428685764301 ) ) ;
#2881 = ORIENTED_EDGE ( 'NONE', *, *, #8613, .T. ) ;
#2882 = CARTESIAN_POINT ( 'NONE',  ( -0.7401821875142703400, 4.673326407553649808, 13.57999999999999652 ) ) ;
#2883 = DIRECTION ( 'NONE',  ( -0.000000000000000000, -0.000000000000000000, 1.000000000000000000 ) ) ;
#2884 = VECTOR ( 'NONE', #9351, 1000.000000000000000 ) ;
#2885 = CARTESIAN_POINT ( 'NONE',  ( -3.345732310141667831, 3.345732310141653620, 2.099999999999999201 ) ) ;
#2886 = VECTOR ( 'NONE', #1116, 1000.000000000000000 ) ;
#2887 = CARTESIAN_POINT ( 'NONE',  ( -1.500000000000000000, -12.13397459621556607, -2.791666666666666519 ) ) ;
#2888 = ORIENTED_EDGE ( 'NONE', *, *, #2029, .T. ) ;
#2889 = VECTOR ( 'NONE', #6206, 1000.000000000000000 ) ;
#2890 = VECTOR ( 'NONE', #3092, 1000.000000000000000 ) ;
#2891 = VERTEX_POINT ( 'NONE', #9896 ) ;
#2892 = DIRECTION ( 'NONE',  ( 5.204170427930421283E-15, 6.018531076210112041E-31, 1.000000000000000000 ) ) ;
#2893 = CYLINDRICAL_SURFACE ( 'NONE', #5265, 2.000000000000001776 ) ;
#2894 = VECTOR ( 'NONE', #9353, 1000.000000000000000 ) ;
#2895 = CARTESIAN_POINT ( 'NONE',  ( 10.00000000000000000, -2.417132211460011337, -8.149077976821821778 ) ) ;
#2896 = ORIENTED_EDGE ( 'NONE', *, *, #2906, .T. ) ;
#2897 = CARTESIAN_POINT ( 'NONE',  ( -5.726445515403654873, 0.8124729078101847746, 11.21605171672202417 ) ) ;
#2898 = CARTESIAN_POINT ( 'NONE',  ( 5.152728359536493663, 2.625446233515533745, 8.539999999999999147 ) ) ;
#2899 = AXIS2_PLACEMENT_3D ( 'NONE', #1671, #3263, #1882 ) ;
#2900 = LINE ( 'NONE', #3741, #5744 ) ;
#2901 = EDGE_LOOP ( 'NONE', ( #1740, #9429 ) ) ;
#2902 = LINE ( 'NONE', #10225, #31 ) ;
#2903 = PRODUCT_DEFINITION_CONTEXT ( 'detailed design', #9953, 'design' ) ;
#2904 = ORIENTED_EDGE ( 'NONE', *, *, #926, .F. ) ;
#2905 = ADVANCED_FACE ( 'NONE', ( #5051 ), #1031, .T. ) ;
#2906 = EDGE_CURVE ( 'NONE', #2891, #5519, #4952, .T. ) ;
#2907 = SURFACE_SIDE_STYLE ('',( #1210 ) ) ;
#2908 = ORIENTED_EDGE ( 'NONE', *, *, #10395, .T. ) ;
#2909 = FACE_OUTER_BOUND ( 'NONE', #9860, .T. ) ;
#2910 = DIRECTION ( 'NONE',  ( -1.000000000000000000, -0.000000000000000000, -0.000000000000000000 ) ) ;
#2911 = VERTEX_POINT ( 'NONE', #4899 ) ;
#2912 = PLANE ( 'NONE',  #4381 ) ;
#2913 = EDGE_CURVE ( 'NONE', #1944, #8403, #3361, .T. ) ;
#2914 = CARTESIAN_POINT ( 'NONE',  ( 1.300000000000000044, -0.7390083445627200209, 1.280000000000001137 ) ) ;
#2915 = CARTESIAN_POINT ( 'NONE',  ( -3.279728542977953687, 3.411736077305369541, 6.703948283277976650 ) ) ;
#2916 = ORIENTED_EDGE ( 'NONE', *, *, #7531, .F. ) ;
#2917 = CARTESIAN_POINT ( 'NONE',  ( 1.500000000000000222, -13.00000000000000533, -2.062500001365593416 ) ) ;
#2918 = CARTESIAN_POINT ( 'NONE',  ( -1.499999999999999778, -12.13397459621556784, -0.3541666680322601013 ) ) ;
#2919 =( BOUNDED_CURVE ( )  B_SPLINE_CURVE ( 2, ( #6653, #4319, #4966, #7463, #3377, #5803, #1095 ),
 .UNSPECIFIED., .F., .T. ) 
 B_SPLINE_CURVE_WITH_KNOTS ( ( 3, 2, 2, 3 ),
 ( 0.8333333333333332593, 0.8611111111111110494, 0.8888888888888888395, 0.9166666666666666297 ),
 .UNSPECIFIED. ) 
 CURVE ( )  GEOMETRIC_REPRESENTATION_ITEM ( )  RATIONAL_B_SPLINE_CURVE ( ( 1.000000000000000444, 0.8660254037844381525, 1.000000000000000000, 0.8660254037844387076, 1.000000000000000000, 0.8660254037844387076, 1.000000000000000000 ) ) 
 REPRESENTATION_ITEM ( '' )  );
#2920 = DIRECTION ( 'NONE',  ( -1.000000000000000000, -0.000000000000000000, -0.000000000000000000 ) ) ;
#2921 = CARTESIAN_POINT ( 'NONE',  ( -5.432285873273256627, -0.8603895577212797852, 12.87999999999999901 ) ) ;
#2922 = LINE ( 'NONE', #4605, #6089 ) ;
#2923 = CARTESIAN_POINT ( 'NONE',  ( 50.00005079999999680, 0.000000000000000000, 0.000000000000000000 ) ) ;
#2924 = CARTESIAN_POINT ( 'NONE',  ( 0.000000000000000000, -10.00000000000000000, -12.00000000000000000 ) ) ;
#2925 = ADVANCED_FACE ( 'NONE', ( #136 ), #2519, .T. ) ;
#2926 = CARTESIAN_POINT ( 'NONE',  ( -29.99999999999998934, 0.000000000000000000, 0.000000000000000000 ) ) ;
#2927 = CARTESIAN_POINT ( 'NONE',  ( 0.7401821875142697849, -4.673326407553650697, 0.9799999999999997602 ) ) ;
#2928 = CARTESIAN_POINT ( 'NONE',  ( -2.607672531582950546E-16, -14.41955080893447416, -0.3437500006827965415 ) ) ;
#2929 = CARTESIAN_POINT ( 'NONE',  ( 2.708615832122949652, 5.110351332421781301, 4.463948283277976437 ) ) ;
#2930 = CARTESIAN_POINT ( 'NONE',  ( 1.229367062500000163, -13.00000000000000533, 0.2812499993172035695 ) ) ;
#2931 = VERTEX_POINT ( 'NONE', #1238 ) ;
#2932 = CIRCLE ( 'NONE', #5633, 2.750000000000000000 ) ;
#2933 = DIRECTION ( 'NONE',  ( 1.000000000000000000, 0.000000000000000000, 0.000000000000000000 ) ) ;
#2934 = EDGE_CURVE ( 'NONE', #6822, #5643, #6618, .T. ) ;
#2935 = CARTESIAN_POINT ( 'NONE',  ( 10.00000000000000000, 3.771202944355774189, -4.982773259188334691 ) ) ;
#2936 = DIRECTION ( 'NONE',  ( 1.000000000000000000, -0.000000000000000000, -0.000000000000000000 ) ) ;
#2937 = EDGE_CURVE ( 'NONE', #9930, #8882, #2829, .T. ) ;
#2938 = FACE_OUTER_BOUND ( 'NONE', #7013, .T. ) ;
#2939 = VERTEX_POINT ( 'NONE', #4514 ) ;
#2940 = LINE ( 'NONE', #4570, #7603 ) ;
#2941 = AXIS2_PLACEMENT_3D ( 'NONE', #2970, #4653, #632 ) ;
#2942 = DIRECTION ( 'NONE',  ( 0.3420201433256627732, -0.9396926207859105373, 0.000000000000000000 ) ) ;
#2943 = CARTESIAN_POINT ( 'NONE',  ( -2.122056237541221968, 3.969226411068977889, 14.43605171672202125 ) ) ;
#2944 = CARTESIAN_POINT ( 'NONE',  ( 1.229367062499999719, -13.70977540446724063, -1.885416667349463449 ) ) ;
#2945 = ORIENTED_EDGE ( 'NONE', *, *, #1624, .F. ) ;
#2946 = ORIENTED_EDGE ( 'NONE', *, *, #4300, .F. ) ;
#2947 =( GEOMETRIC_REPRESENTATION_CONTEXT ( 3 ) GLOBAL_UNCERTAINTY_ASSIGNED_CONTEXT ( ( #3643 ) ) GLOBAL_UNIT_ASSIGNED_CONTEXT ( ( #1, #6456, #4125 ) ) REPRESENTATION_CONTEXT ( 'NONE', 'WORKASPACE' ) );
#2948 = EDGE_CURVE ( 'NONE', #7840, #3946, #2400, .T. ) ;
#2949 = FACE_OUTER_BOUND ( 'NONE', #8605, .T. ) ;
#2950 = CARTESIAN_POINT ( 'NONE',  ( 1.999999999999987121, 15.00000000000000355, 4.000000000000008882 ) ) ;
#2951 = EDGE_LOOP ( 'NONE', ( #673, #7930 ) ) ;
#2952 = CARTESIAN_POINT ( 'NONE',  ( -0.9968613283357868893, 5.697241258616382531, 8.976051716722020402 ) ) ;
#2953 = CARTESIAN_POINT ( 'NONE',  ( -2.000000000000000000, 0.000000000000000000, 0.000000000000000000 ) ) ;
#2954 = ORIENTED_EDGE ( 'NONE', *, *, #8671, .F. ) ;
#2955 = CARTESIAN_POINT ( 'NONE',  ( 1.060575238724907038E-16, -11.26794919243112680, -1.437500001365593416 ) ) ;
#2956 = ORIENTED_EDGE ( 'NONE', *, *, #8576, .T. ) ;
#2957 = SHAPE_REPRESENTATION_RELATIONSHIP ( 'NONE' , 'NONE' ,  #13, #2960 ) ;
#2958 = VERTEX_POINT ( 'NONE', #1986 ) ;
#2959 = DIRECTION ( 'NONE',  ( 1.000000000000000000, 0.000000000000000000, 0.000000000000000000 ) ) ;
#2960 = ADVANCED_BREP_SHAPE_REPRESENTATION ( '', ( #4712, #2101 ), #6502 ) ;
#2961 = CARTESIAN_POINT ( 'NONE',  ( -13.00000000000000000, 19.99999999999999645, 6.000000000000000000 ) ) ;
#2962 = EDGE_LOOP ( 'NONE', ( #7083, #7502 ) ) ;
#2963 = CIRCLE ( 'NONE', #2828, 6.248999999999999666 ) ;
#2964 = DIRECTION ( 'NONE',  ( 0.000000000000000000, 0.000000000000000000, -1.000000000000000000 ) ) ;
#2965 = CARTESIAN_POINT ( 'NONE',  ( 17.00000000000000000, 19.99999999999999645, -9.000000000000000000 ) ) ;
#2966 = CARTESIAN_POINT ( 'NONE',  ( -2.417848759854264618, 4.940838830814694660, 1.243948283277976463 ) ) ;
#2967 = ORIENTED_EDGE ( 'NONE', *, *, #8249, .F. ) ;
#2968 = VECTOR ( 'NONE', #2751, 1000.000000000000000 ) ;
#2969 = CARTESIAN_POINT ( 'NONE',  ( 7.546553696766195252, -10.00000000000000000, -12.00000000000000000 ) ) ;
#2970 = CARTESIAN_POINT ( 'NONE',  ( 8.000000000000001776, 0.000000000000000000, 0.000000000000000000 ) ) ;
#2971 = AXIS2_PLACEMENT_3D ( 'NONE', #6857, #9204, #7560 ) ;
#2972 = LINE ( 'NONE', #10291, #4628 ) ;
#2973 = CARTESIAN_POINT ( 'NONE',  ( -3.889087296526005044, -3.889087296526019255, 12.59999999999999787 ) ) ;
#2974 = AXIS2_PLACEMENT_3D ( 'NONE', #9218, #3747, #10129 ) ;
#2975 = CYLINDRICAL_SURFACE ( 'NONE', #514, 1.249999999999993339 ) ;
#2976 = CARTESIAN_POINT ( 'NONE',  ( -2.399999999999999911, 0.000000000000000000, 6.999999999999999112 ) ) ;
#2977 = DIRECTION ( 'NONE',  ( 0.000000000000000000, 0.000000000000000000, 1.000000000000000000 ) ) ;
#2978 = AXIS2_PLACEMENT_3D ( 'NONE', #969, #7491, #2508 ) ;
#2979 = DIRECTION ( 'NONE',  ( -1.000000000000000000, -0.000000000000000000, -0.000000000000000000 ) ) ;
#2980 = CARTESIAN_POINT ( 'NONE',  ( 3.181980515339458471, 3.181980515339470461, 8.400000000000000355 ) ) ;
#2981 = CARTESIAN_POINT ( 'NONE',  ( -2.607672531582950546E-16, -14.41955080893447416, 0.1562499993172034585 ) ) ;
#2982 = VECTOR ( 'NONE', #1093, 1000.000000000000000 ) ;
#2983 = CARTESIAN_POINT ( 'NONE',  ( -0.8124729078102072011, 5.726445515403652209, 6.983948283277976010 ) ) ;
#2984 = CARTESIAN_POINT ( 'NONE',  ( 17.58618750323380908, 6.000000000000000000, 0.000000000000000000 ) ) ;
#2985 = AXIS2_PLACEMENT_3D ( 'NONE', #5932, #330, #2820 ) ;
#2986 = EDGE_CURVE ( 'NONE', #4320, #10319, #8330, .T. ) ;
#2987 = ORIENTED_EDGE ( 'NONE', *, *, #8007, .T. ) ;
#2988 = DIRECTION ( 'NONE',  ( 0.000000000000000000, 0.000000000000000000, 1.000000000000000000 ) ) ;
#2989 = DIRECTION ( 'NONE',  ( 0.000000000000000000, -0.4999999999999992784, 0.8660254037844390407 ) ) ;
#2990 = FACE_BOUND ( 'NONE', #6798, .T. ) ;
#2991 = LINE ( 'NONE', #4620, #5759 ) ;
#2992 = ORIENTED_EDGE ( 'NONE', *, *, #2934, .T. ) ;
#2993 = DIRECTION ( 'NONE',  ( -1.000000000000000000, -0.000000000000000000, -0.000000000000000000 ) ) ;
#2994 = DIRECTION ( 'NONE',  ( 0.3420201433256627732, -0.9396926207859105373, 0.000000000000000000 ) ) ;
#2995 = CARTESIAN_POINT ( 'NONE',  ( -2.148092372876330813, -4.215868657802593233, 9.659999999999994813 ) ) ;
#2996 = EDGE_CURVE ( 'NONE', #3003, #8333, #6156, .T. ) ;
#2997 = CARTESIAN_POINT ( 'NONE',  ( -3.181725716174720498E-16, -14.73205080756888385, -2.625000000000000000 ) ) ;
#2998 = EDGE_CURVE ( 'NONE', #5643, #6822, #3740, .T. ) ;
#2999 = ORIENTED_EDGE ( 'NONE', *, *, #2877, .T. ) ;
#3000 = ORIENTED_EDGE ( 'NONE', *, *, #8763, .T. ) ;
#3001 = CARTESIAN_POINT ( 'NONE',  ( -13.00000000000000000, 19.99999999999999645, -9.000000000000000000 ) ) ;
#3002 = CARTESIAN_POINT ( 'NONE',  ( -29.99999999999998934, 34.99999999999999289, -9.000000000000000000 ) ) ;
#3003 = VERTEX_POINT ( 'NONE', #9408 ) ;
#3004 = CARTESIAN_POINT ( 'NONE',  ( -0.9968613283357868893, 5.697241258616382531, 11.77605171672202289 ) ) ;
#3005 = DIRECTION ( 'NONE',  ( -1.000000000000000000, -0.000000000000000000, -0.000000000000000000 ) ) ;
#3006 = EDGE_LOOP ( 'NONE', ( #3032, #421, #7028, #8367 ) ) ;
#3007 = CARTESIAN_POINT ( 'NONE',  ( -0.7499999999999997780, -11.70096189432334555, -1.395833334698926897 ) ) ;
#3008 = EDGE_CURVE ( 'NONE', #2653, #3837, #10448, .T. ) ;
#3009 = ORIENTED_EDGE ( 'NONE', *, *, #5502, .T. ) ;
#3010 = SHAPE_REPRESENTATION_RELATIONSHIP ( 'NONE' , 'NONE' ,  #7608, #6736 ) ;
#3011 = EDGE_LOOP ( 'NONE', ( #7772, #7066, #1257, #3387 ) ) ;
#3012 = DIRECTION ( 'NONE',  ( -0.000000000000000000, -1.000000000000000000, -0.000000000000000000 ) ) ;
#3013 = DIRECTION ( 'NONE',  ( 0.000000000000000000, 0.000000000000000000, 1.000000000000000000 ) ) ;
#3014 = ORIENTED_EDGE ( 'NONE', *, *, #9849, .F. ) ;
#3015 = CARTESIAN_POINT ( 'NONE',  ( 8.000000000000001776, 0.000000000000000000, 0.000000000000000000 ) ) ;
#3016 = CARTESIAN_POINT ( 'NONE',  ( 1.364683531250000303, -13.00000000000000533, 0.07812499965860171536 ) ) ;
#3017 = CARTESIAN_POINT ( 'NONE',  ( -4.023224611898323033, 4.155232146225737111, 1.103948283277976561 ) ) ;
#3018 = ORIENTED_EDGE ( 'NONE', *, *, #859, .F. ) ;
#3019 = DIRECTION ( 'NONE',  ( -1.000000000000000000, -0.000000000000000000, 0.000000000000000000 ) ) ;
#3020 = LINE ( 'NONE', #10347, #7178 ) ;
#3021 = DIRECTION ( 'NONE',  ( 0.000000000000000000, 0.8660254037844380415, -0.5000000000000009992 ) ) ;
#3022 = CARTESIAN_POINT ( 'NONE',  ( -5.711843387010019590, 0.9046671180729746187, 13.01999999999999602 ) ) ;
#3023 = DIRECTION ( 'NONE',  ( 0.000000000000000000, -1.000000000000000000, 0.000000000000000000 ) ) ;
#3024 = CARTESIAN_POINT ( 'NONE',  ( 1.300000000000000044, 1.478016689125442484, -1.626303258728256651E-15 ) ) ;
#3025 = CARTESIAN_POINT ( 'NONE',  ( -2.000000000000000000, 0.000000000000000000, 0.000000000000000000 ) ) ;
#3026 = FACE_OUTER_BOUND ( 'NONE', #355, .T. ) ;
#3027 = CARTESIAN_POINT ( 'NONE',  ( -2.148092372876330813, -4.215868657802593233, 4.059999999999999609 ) ) ;
#3028 = CIRCLE ( 'NONE', #9128, 3.000000000000000000 ) ;
#3029 = CARTESIAN_POINT ( 'NONE',  ( -1.229367062500000163, -13.00000000000000533, -2.093750000682796930 ) ) ;
#3030 = CARTESIAN_POINT ( 'NONE',  ( -0.8124729078102072011, 5.726445515403652209, 9.783948283277975833 ) ) ;
#3031 = LINE ( 'NONE', #4038, #3771 ) ;
#3032 = ORIENTED_EDGE ( 'NONE', *, *, #5450, .F. ) ;
#3033 = CONTEXT_DEPENDENT_SHAPE_REPRESENTATION ( #3438, #1583 ) ;
#3034 = EDGE_CURVE ( 'NONE', #5902, #10253, #1115, .T. ) ;
#3035 = DIRECTION ( 'NONE',  ( -0.000000000000000000, -0.000000000000000000, 1.000000000000000000 ) ) ;
#3036 = VECTOR ( 'NONE', #5680, 1000.000000000000000 ) ;
#3037 = CARTESIAN_POINT ( 'NONE',  ( -2.000000000000000000, 7.008469740302810891, 2.257469275785291440 ) ) ;
#3038 = VECTOR ( 'NONE', #6715, 1000.000000000000000 ) ;
#3039 = DIRECTION ( 'NONE',  ( -1.156482317317871478E-16, 1.000000000000000000, 0.000000000000000000 ) ) ;
#3040 = CARTESIAN_POINT ( 'NONE',  ( 10.00000000000000000, 8.265874651078018331, 1.981241088980807419 ) ) ;
#3041 = ORIENTED_EDGE ( 'NONE', *, *, #6947, .F. ) ;
#3042 = AXIS2_PLACEMENT_3D ( 'NONE', #2566, #7977, #5575 ) ;
#3043 = EDGE_CURVE ( 'NONE', #5372, #292, #2879, .T. ) ;
#3044 = DIRECTION ( 'NONE',  ( 5.204170427930421283E-15, 6.018531076210112041E-31, 1.000000000000000000 ) ) ;
#3045 = AXIS2_PLACEMENT_3D ( 'NONE', #9437, #9271, #8531 ) ;
#3046 = CARTESIAN_POINT ( 'NONE',  ( 2.042957248827968808, -4.009529358847652603, 9.240000000000000213 ) ) ;
#3047 =( GEOMETRIC_REPRESENTATION_CONTEXT ( 3 ) GLOBAL_UNCERTAINTY_ASSIGNED_CONTEXT ( ( #6318 ) ) GLOBAL_UNIT_ASSIGNED_CONTEXT ( ( #3624, #9954, #10058 ) ) REPRESENTATION_CONTEXT ( 'NONE', 'WORKASPACE' ) );
#3048 = CARTESIAN_POINT ( 'NONE',  ( 1.500000000000000222, -13.00000000000000533, -2.500000000000000000 ) ) ;
#3049 = VERTEX_POINT ( 'NONE', #1289 ) ;
#3050 = ORIENTED_EDGE ( 'NONE', *, *, #5944, .F. ) ;
#3051 = CARTESIAN_POINT ( 'NONE',  ( 0.000000000000000000, -13.00000000000000533, -3.000000000000000000 ) ) ;
#3052 = SURFACE_STYLE_FILL_AREA ( #7877 ) ;
#3053 = ORIENTED_EDGE ( 'NONE', *, *, #1059, .F. ) ;
#3054 = EDGE_CURVE ( 'NONE', #4330, #2931, #4565, .T. ) ;
#3055 = CARTESIAN_POINT ( 'NONE',  ( -5.418398423912711870, -0.9480714621563917088, 11.07605171672202182 ) ) ;
#3056 = EDGE_CURVE ( 'NONE', #3589, #9435, #8569, .T. ) ;
#3057 = CARTESIAN_POINT ( 'NONE',  ( 1.272613240716556016, -10.02539999999999942, 0.000000000000000000 ) ) ;
#3058 = PRESENTATION_STYLE_ASSIGNMENT (( #7775 ) ) ;
#3059 = ORIENTED_EDGE ( 'NONE', *, *, #7, .T. ) ;
#3060 = CARTESIAN_POINT ( 'NONE',  ( -2.000000000000000000, -5.848742439617878652, -6.167836887841048110 ) ) ;
#3061 = CARTESIAN_POINT ( 'NONE',  ( 5.418398423912711870, 0.9480714621563913758, 12.47605171672202218 ) ) ;
#3062 = VECTOR ( 'NONE', #7711, 1000.000000000000000 ) ;
#3063 = EDGE_LOOP ( 'NONE', ( #7234, #9246, #6794, #2104 ) ) ;
#3064 = CARTESIAN_POINT ( 'NONE',  ( 8.000000000000001776, 0.000000000000000000, 0.000000000000000000 ) ) ;
#3065 = LINE ( 'NONE', #1638, #2542 ) ;
#3066 = AXIS2_PLACEMENT_3D ( 'NONE', #8718, #7287, #9471 ) ;
#3067 = ORIENTED_EDGE ( 'NONE', *, *, #6295, .F. ) ;
#3068 = ADVANCED_FACE ( 'NONE', ( #3618 ), #6847, .F. ) ;
#3069 = PLANE ( 'NONE',  #10326 ) ;
#3070 = DIRECTION ( 'NONE',  ( 0.000000000000000000, -0.000000000000000000, 1.000000000000000000 ) ) ;
#3071 = CARTESIAN_POINT ( 'NONE',  ( -3.951860609387083834, -3.826313983664940466, 8.803948283277977183 ) ) ;
#3072 = ORIENTED_EDGE ( 'NONE', *, *, #3676, .F. ) ;
#3073 = CARTESIAN_POINT ( 'NONE',  ( -1.500000000000000222, -13.00000000000000533, -2.312500001365593860 ) ) ;
#3074 = LINE ( 'NONE', #8590, #2604 ) ;
#3075 = EDGE_LOOP ( 'NONE', ( #3776, #3849, #1670, #7828 ) ) ;
#3076 = CARTESIAN_POINT ( 'NONE',  ( 10.00000000000000000, -7.063614741696270016, 2.343061888689530026 ) ) ;
#3077 = FACE_OUTER_BOUND ( 'NONE', #4805, .T. ) ;
#3078 = CARTESIAN_POINT ( 'NONE',  ( 30.00000000000001066, 35.00000000000001421, -6.000000000000000000 ) ) ;
#3079 = EDGE_CURVE ( 'NONE', #3593, #4169, #5156, .T. ) ;
#3080 = DIRECTION ( 'NONE',  ( 0.000000000000000000, 1.000000000000000000, 0.000000000000000000 ) ) ;
#3081 = CARTESIAN_POINT ( 'NONE',  ( 8.000000000000001776, 2.871924938129970517, -6.435996203144478400 ) ) ;
#3082 = CARTESIAN_POINT ( 'NONE',  ( 3.345732310141667387, -3.345732310141653620, 3.499999999999998668 ) ) ;
#3083 = CARTESIAN_POINT ( 'NONE',  ( -1.229367062500000163, -13.00000000000000533, -0.4687500006827967081 ) ) ;
#3084 = CARTESIAN_POINT ( 'NONE',  ( 0.9480714621563713917, 5.418398423912717199, 9.923948283277976401 ) ) ;
#3085 = CARTESIAN_POINT ( 'NONE',  ( -5.999999999999999112, -27.00000000000000711, -4.000000000000000000 ) ) ;
#3086 = ORIENTED_EDGE ( 'NONE', *, *, #7400, .F. ) ;
#3087 = PRODUCT_CONTEXT ( 'NONE', #9064, 'mechanical' ) ;
#3088 = LINE ( 'NONE', #4669, #5327 ) ;
#3089 = LINE ( 'NONE', #8706, #2982 ) ;
#3090 = EDGE_LOOP ( 'NONE', ( #512, #1108, #3371, #1338 ) ) ;
#3091 = CARTESIAN_POINT ( 'NONE',  ( 0.000000000000000000, 6.000000000000000000, -12.00000000000000000 ) ) ;
#3092 = DIRECTION ( 'NONE',  ( 0.3420201433256627732, 0.9396926207859105373, -0.000000000000000000 ) ) ;
#3093 = VERTEX_POINT ( 'NONE', #6105 ) ;
#3094 =( NAMED_UNIT ( * ) SI_UNIT ( $, .STERADIAN. ) SOLID_ANGLE_UNIT ( ) );
#3095 = FILL_AREA_STYLE ('',( #9575 ) ) ;
#3096 = CARTESIAN_POINT ( 'NONE',  ( -0.7039550926810301812, -4.444597532678121965, 9.519999999999999574 ) ) ;
#3097 = APPLICATION_CONTEXT ( 'automotive_design' ) ;
#3098 = VECTOR ( 'NONE', #1159, 1000.000000000000000 ) ;
#3099 = CARTESIAN_POINT ( 'NONE',  ( 1.500000000000000000, -13.86602540378444459, -2.041666666666666963 ) ) ;
#3100 = ORIENTED_EDGE ( 'NONE', *, *, #3333, .T. ) ;
#3101 = EDGE_CURVE ( 'NONE', #10205, #8915, #5315, .T. ) ;
#3102 = EDGE_LOOP ( 'NONE', ( #6920, #6805, #831, #7243 ) ) ;
#3103 = CARTESIAN_POINT ( 'NONE',  ( 27.00000000000001066, 35.00000000000001421, -5.999999999999999112 ) ) ;
#3104 = AXIS2_PLACEMENT_3D ( 'NONE', #1495, #10475, #8077 ) ;
#3105 = VERTEX_POINT ( 'NONE', #7598 ) ;
#3106 = CARTESIAN_POINT ( 'NONE',  ( -5.418398423912711870, -0.9480714621563917088, 8.276051716722021112 ) ) ;
#3107 = CARTESIAN_POINT ( 'NONE',  ( 3.099999999999998757, 0.000000000000000000, 0.000000000000000000 ) ) ;
#3108 = EDGE_LOOP ( 'NONE', ( #743, #8169, #2482 ) ) ;
#3109 = CARTESIAN_POINT ( 'NONE',  ( -29.99999999999998934, 34.99999999999999289, 9.000000000000000000 ) ) ;
#3110 = CARTESIAN_POINT ( 'NONE',  ( 2.576046737280769605, -4.860232935257343456, 10.23605171672202374 ) ) ;
#3111 = VERTEX_POINT ( 'NONE', #10000 ) ;
#3112 = ADVANCED_FACE ( 'NONE', ( #3671 ), #344, .T. ) ;
#3113 = ORIENTED_EDGE ( 'NONE', *, *, #7728, .F. ) ;
#3114 = DIRECTION ( 'NONE',  ( 0.000000000000000000, 0.000000000000000000, 1.000000000000000000 ) ) ;
#3115 = LINE ( 'NONE', #8788, #675 ) ;
#3116 = EDGE_LOOP ( 'NONE', ( #2779, #5943 ) ) ;
#3117 = CARTESIAN_POINT ( 'NONE',  ( 30.00000000000001066, -34.99999999999999289, -9.000000000000000000 ) ) ;
#3118 = DIRECTION ( 'NONE',  ( 0.000000000000000000, 2.602085213965210642E-15, -1.000000000000000000 ) ) ;
#3119 = CARTESIAN_POINT ( 'NONE',  ( -5.195105386651219348, -2.542276634908102295, 3.343948283277975886 ) ) ;
#3121 = ORIENTED_EDGE ( 'NONE', *, *, #10406, .T. ) ;
#3120 = VECTOR ( 'NONE', #6352, 1000.000000000000000 ) ;
#3122 = CARTESIAN_POINT ( 'NONE',  ( -0.7500000000000007772, -14.29903810567666156, -1.229166668032260157 ) ) ;
#3123 = DIRECTION ( 'NONE',  ( -0.000000000000000000, -0.000000000000000000, -1.000000000000000000 ) ) ;
#3124 = EDGE_CURVE ( 'NONE', #4718, #5808, #9764, .T. ) ;
#3125 = EDGE_CURVE ( 'NONE', #7252, #4491, #1627, .T. ) ;
#3126 = PRESENTATION_LAYER_ASSIGNMENT (  '', '', ( #1776 ) ) ;
#3127 = EDGE_LOOP ( 'NONE', ( #5434, #156, #2381, #3839 ) ) ;
#3128 = CARTESIAN_POINT ( 'NONE',  ( 10.00000000000000000, -2.834406817834849601, -8.013497238472808704 ) ) ;
#3129 = CARTESIAN_POINT ( 'NONE',  ( -0.7499999999999997780, -11.70096189432334555, -2.333333333333333481 ) ) ;
#3130 = PLANE ( 'NONE',  #1343 ) ;
#3131 = PLANE ( 'NONE',  #7897 ) ;
#3132 = DIRECTION ( 'NONE',  ( 0.000000000000000000, 0.000000000000000000, 1.000000000000000000 ) ) ;
#3133 = CARTESIAN_POINT ( 'NONE',  ( 4.673326407553653361, -0.7401821875142523544, 8.820000000000000284 ) ) ;
#3134 = CARTESIAN_POINT ( 'NONE',  ( -1.229367062500000385, -13.70977540446723886, -1.052083334016129967 ) ) ;
#3135 = CARTESIAN_POINT ( 'NONE',  ( -4.860232935257354114, 2.576046737280751842, 12.16394828327797661 ) ) ;
#3136 = EDGE_CURVE ( 'NONE', #5844, #1096, #9248, .T. ) ;
#3137 = DIRECTION ( 'NONE',  ( 0.3420201433256627732, -0.9396926207859105373, 0.000000000000000000 ) ) ;
#3138 = AXIS2_PLACEMENT_3D ( 'NONE', #2219, #4807, #3114 ) ;
#3139 = VERTEX_POINT ( 'NONE', #10259 ) ;
#3140 = SHAPE_DEFINITION_REPRESENTATION ( #4788, #5100 ) ;
#3141 = CARTESIAN_POINT ( 'NONE',  ( -2.000000000000019096, 35.00000000000000000, -6.000000000000000000 ) ) ;
#3142 = CARTESIAN_POINT ( 'NONE',  ( 3.000000000000000888, 2.750000000000000000, 0.000000000000000000 ) ) ;
#3143 = ORIENTED_EDGE ( 'NONE', *, *, #10256, .T. ) ;
#3144 = CARTESIAN_POINT ( 'NONE',  ( 0.000000000000000000, -4.000000000000000000, -2.000000000000000000 ) ) ;
#3145 = CYLINDRICAL_SURFACE ( 'NONE', #2212, 6.248999999999999666 ) ;
#3146 = LINE ( 'NONE', #814, #8969 ) ;
#3147 = VECTOR ( 'NONE', #406, 1000.000000000000000 ) ;
#3148 = DIRECTION ( 'NONE',  ( -1.000000000000000000, -1.156482317317871478E-16, -0.000000000000000000 ) ) ;
#3149 = CARTESIAN_POINT ( 'NONE',  ( 25.00000000000000000, 0.000000000000000000, -12.00000000000000000 ) ) ;
#3150 = VECTOR ( 'NONE', #1933, 1000.000000000000000 ) ;
#3151 = CARTESIAN_POINT ( 'NONE',  ( 3.244753828200538148, 3.119207202478391672, -0.9960517167220231949 ) ) ;
#3152 = PRODUCT_DEFINITION_CONTEXT ( 'detailed design', #2357, 'design' ) ;
#3153 = CARTESIAN_POINT ( 'NONE',  ( -0.7499999999999997780, -11.70096189432334555, -2.333333333333333481 ) ) ;
#3154 = ORIENTED_EDGE ( 'NONE', *, *, #9656, .T. ) ;
#3155 = ORIENTED_EDGE ( 'NONE', *, *, #1957, .F. ) ;
#3156 = LINE ( 'NONE', #4848, #2725 ) ;
#3157 =( NAMED_UNIT ( * ) SI_UNIT ( $, .STERADIAN. ) SOLID_ANGLE_UNIT ( ) );
#3158 = ORIENTED_EDGE ( 'NONE', *, *, #5322, .F. ) ;
#3159 = DIRECTION ( 'NONE',  ( 0.3420201433256627732, 0.9396926207859105373, 0.000000000000000000 ) ) ;
#3160 = DIRECTION ( 'NONE',  ( 1.000000000000000000, 0.000000000000000000, 0.000000000000000000 ) ) ;
#3161 = VERTEX_POINT ( 'NONE', #2300 ) ;
#3162 = DIRECTION ( 'NONE',  ( 0.000000000000000000, 0.000000000000000000, 1.000000000000000000 ) ) ;
#3163 = CARTESIAN_POINT ( 'NONE',  ( 5.110351332421769754, 2.708615832122969191, 9.536051716722020899 ) ) ;
#3164 = ORIENTED_EDGE ( 'NONE', *, *, #9984, .F. ) ;
#3165 =( NAMED_UNIT ( * ) PLANE_ANGLE_UNIT ( ) SI_UNIT ( $, .RADIAN. ) );
#3166 = ORIENTED_EDGE ( 'NONE', *, *, #4976, .F. ) ;
#3167 = DIRECTION ( 'NONE',  ( 0.3420201433256627732, 0.9396926207859105373, 0.000000000000000000 ) ) ;
#3168 = DIRECTION ( 'NONE',  ( 0.000000000000000000, 0.000000000000000000, 1.000000000000000000 ) ) ;
#3169 = VERTEX_POINT ( 'NONE', #4725 ) ;
#3170 = CARTESIAN_POINT ( 'NONE',  ( -3.889087296526005044, -3.889087296526019255, 6.999999999999999112 ) ) ;
#3171 = DIRECTION ( 'NONE',  ( 1.000000000000000000, 0.000000000000000000, 0.000000000000000000 ) ) ;
#3172 = CARTESIAN_POINT ( 'NONE',  ( -4.023224611898323033, 4.155232146225737111, 3.903948283277975939 ) ) ;
#3173 = ORIENTED_EDGE ( 'NONE', *, *, #9523, .F. ) ;
#3174 = CARTESIAN_POINT ( 'NONE',  ( -3.181725716174720498E-16, -14.73205080756888385, -1.687500001365593638 ) ) ;
#3175 = ADVANCED_FACE ( 'NONE', ( #3995 ), #1394, .T. ) ;
#3176 = CARTESIAN_POINT ( 'NONE',  ( -1.500000000000000222, -13.00000000000000533, -1.312500001365593416 ) ) ;
#3177 =( NAMED_UNIT ( * ) PLANE_ANGLE_UNIT ( ) SI_UNIT ( $, .RADIAN. ) );
#3178 = ORIENTED_EDGE ( 'NONE', *, *, #3101, .F. ) ;
#3179 = PRODUCT_DEFINITION_SHAPE ( 'NONE', 'NONE',  #3345 ) ;
#3180 = CARTESIAN_POINT ( 'NONE',  ( 18.40512053033274853, 3.750000000000000000, -12.00000000000000000 ) ) ;
#3181 = LINE ( 'NONE', #9768, #7297 ) ;
#3182 = CARTESIAN_POINT ( 'NONE',  ( 4.000000000000000888, -2.834406817834849601, -8.013497238472808704 ) ) ;
#3183 = DIRECTION ( 'NONE',  ( 0.000000000000000000, -1.000000000000000000, -0.000000000000000000 ) ) ;
#3184 = PLANE ( 'NONE',  #155 ) ;
#3185 = CARTESIAN_POINT ( 'NONE',  ( -2.148092372876330813, -4.215868657802593233, 6.859999999999999432 ) ) ;
#3186 = ADVANCED_FACE ( 'NONE', ( #6372 ), #4786, .F. ) ;
#3187 = VERTEX_POINT ( 'NONE', #8708 ) ;
#3188 = ADVANCED_FACE ( 'NONE', ( #8762 ), #3196, .T. ) ;
#3189 = CARTESIAN_POINT ( 'NONE',  ( 1.229367062499999719, -13.70977540446724063, -0.8854166673494634487 ) ) ;
#3190 = CARTESIAN_POINT ( 'NONE',  ( 4.860232935257354114, -2.576046737280751842, 7.963948283277976437 ) ) ;
#3191 = CYLINDRICAL_SURFACE ( 'NONE', #1404, 3.000000000000000000 ) ;
#3192 = ORIENTED_EDGE ( 'NONE', *, *, #2129, .T. ) ;
#3193 = DIRECTION ( 'NONE',  ( 0.3420201433256627732, 0.9396926207859105373, -0.000000000000000000 ) ) ;
#3194 = FACE_OUTER_BOUND ( 'NONE', #8679, .T. ) ;
#3195 = ORIENTED_EDGE ( 'NONE', *, *, #796, .T. ) ;
#3196 = CYLINDRICAL_SURFACE ( 'NONE', #6525, 1.500000000000000222 ) ;
#3197 = DIRECTION ( 'NONE',  ( 1.000000000000000000, 0.000000000000000000, -0.000000000000000000 ) ) ;
#3198 = DIRECTION ( 'NONE',  ( 0.000000000000000000, 0.000000000000000000, 1.000000000000000000 ) ) ;
#3199 = EDGE_CURVE ( 'NONE', #3641, #2001, #9519, .T. ) ;
#3200 = FACE_OUTER_BOUND ( 'NONE', #6548, .T. ) ;
#3201 = LINE ( 'NONE', #3149, #6256 ) ;
#3202 = CARTESIAN_POINT ( 'NONE',  ( 0.7401821875142697849, -4.673326407553650697, 9.379999999999995453 ) ) ;
#3203 = CARTESIAN_POINT ( 'NONE',  ( -1.500000000000000222, -13.00000000000000533, -1.250000000000000000 ) ) ;
#3204 = AXIS2_PLACEMENT_3D ( 'NONE', #4086, #2396, #4825 ) ;
#3205 = ORIENTED_EDGE ( 'NONE', *, *, #3199, .T. ) ;
#3206 = AXIS2_PLACEMENT_3D ( 'NONE', #6980, #5548, #10184 ) ;
#3207 = ORIENTED_EDGE ( 'NONE', *, *, #9955, .F. ) ;
#3208 = CARTESIAN_POINT ( 'NONE',  ( -2.000000000000000000, -8.497168642645966941, 0.2193742428684610779 ) ) ;
#3209 = ORIENTED_EDGE ( 'NONE', *, *, #5251, .T. ) ;
#3210 = FACE_BOUND ( 'NONE', #7559, .T. ) ;
#3211 = DIRECTION ( 'NONE',  ( 1.000000000000000000, 0.000000000000000000, 0.000000000000000000 ) ) ;
#3212 = ORIENTED_EDGE ( 'NONE', *, *, #2860, .F. ) ;
#3213 = CARTESIAN_POINT ( 'NONE',  ( -5.418398423912711870, -0.9480714621563917088, 13.87605171672202253 ) ) ;
#3214 = ORIENTED_EDGE ( 'NONE', *, *, #8056, .T. ) ;
#3215 = SURFACE_STYLE_USAGE ( .BOTH. , #2372 ) ;
#3216 = VECTOR ( 'NONE', #1587, 1000.000000000000000 ) ;
#3217 = CARTESIAN_POINT ( 'NONE',  ( 13.83898384071655840, -10.02539999999999942, -12.00000000000000000 ) ) ;
#3218 = AXIS2_PLACEMENT_3D ( 'NONE', #1677, #8203, #6490 ) ;
#3219 = CARTESIAN_POINT ( 'NONE',  ( -2.000000000000000000, -7.009698679648292519, 0.7308381473896652381 ) ) ;
#3220 = ORIENTED_EDGE ( 'NONE', *, *, #9614, .F. ) ;
#3221 = CARTESIAN_POINT ( 'NONE',  ( 0.9046671180729951578, -5.711843387010016926, 0.9799999999999997602 ) ) ;
#3222 = DIRECTION ( 'NONE',  ( -1.000000000000000000, -0.000000000000000000, -0.000000000000000000 ) ) ;
#3223 = CARTESIAN_POINT ( 'NONE',  ( -5.697241258616385196, 0.9968613283357647958, 9.223948283277977112 ) ) ;
#3224 = ORIENTED_EDGE ( 'NONE', *, *, #1292, .F. ) ;
#3225 = VECTOR ( 'NONE', #6435, 1000.000000000000000 ) ;
#3226 = CARTESIAN_POINT ( 'NONE',  ( 1.060575238724907038E-16, -11.26794919243112680, -0.4375000013655937492 ) ) ;
#3227 = EDGE_CURVE ( 'NONE', #6924, #1894, #1503, .T. ) ;
#3228 = VECTOR ( 'NONE', #2942, 1000.000000000000000 ) ;
#3229 = VECTOR ( 'NONE', #631, 1000.000000000000000 ) ;
#3230 = ORIENTED_EDGE ( 'NONE', *, *, #3307, .T. ) ;
#3231 = VECTOR ( 'NONE', #2651, 1000.000000000000000 ) ;
#3232 = PLANE ( 'NONE',  #7189 ) ;
#3233 = VECTOR ( 'NONE', #9792, 1000.000000000000000 ) ;
#3234 = EDGE_CURVE ( 'NONE', #1747, #2210, #597, .T. ) ;
#3235 = CARTESIAN_POINT ( 'NONE',  ( 14.44459485323380576, -10.00000000000000000, 0.000000000000000000 ) ) ;
#3236 = FACE_OUTER_BOUND ( 'NONE', #4534, .T. ) ;
#3237 = CARTESIAN_POINT ( 'NONE',  ( -17.00000000000000000, 19.99999999999999645, -9.000000000000000000 ) ) ;
#3238 = VECTOR ( 'NONE', #4691, 1000.000000000000000 ) ;
#3239 = DIRECTION ( 'NONE',  ( 0.000000000000000000, 0.000000000000000000, 1.000000000000000000 ) ) ;
#3240 = CARTESIAN_POINT ( 'NONE',  ( 4.009529358847659708, -2.042957248827953709, 11.75999999999999979 ) ) ;
#3241 = VERTEX_POINT ( 'NONE', #6419 ) ;
#3242 = DIRECTION ( 'NONE',  ( 0.000000000000000000, -1.000000000000000000, 0.000000000000000000 ) ) ;
#3243 = VECTOR ( 'NONE', #929, 1000.000000000000000 ) ;
#3244 = CARTESIAN_POINT ( 'NONE',  ( -4.900535883036028828, 2.496947748567499126, 1.959999999999999964 ) ) ;
#3245 = DIRECTION ( 'NONE',  ( 0.000000000000000000, 0.000000000000000000, 1.000000000000000000 ) ) ;
#3246 = PRODUCT_CONTEXT ( 'NONE', #3297, 'mechanical' ) ;
#3247 = LINE ( 'NONE', #2297, #7869 ) ;
#3248 = ADVANCED_FACE ( 'NONE', ( #5573, #2990 ), #10307, .F. ) ;
#3249 = CARTESIAN_POINT ( 'NONE',  ( 0.7499999999999991118, -14.29903810567666333, -1.645833334698926675 ) ) ;
#3250 = CARTESIAN_POINT ( 'NONE',  ( 1.500000000000000222, -13.00000000000000533, -0.06250000136559345776 ) ) ;
#3251 = FACE_OUTER_BOUND ( 'NONE', #2470, .T. ) ;
#3252 = DIRECTION ( 'NONE',  ( -1.000000000000000000, 0.000000000000000000, -0.000000000000000000 ) ) ;
#3253 = DIRECTION ( 'NONE',  ( -1.000000000000000000, -0.000000000000000000, -0.000000000000000000 ) ) ;
#3254 = CARTESIAN_POINT ( 'NONE',  ( -5.999999999999999112, -27.00000000000000711, 3.000000000000000000 ) ) ;
#3255 = CARTESIAN_POINT ( 'NONE',  ( 2.231261971483764484, 4.173491630687871101, 1.663948283277976392 ) ) ;
#3256 = UNCERTAINTY_MEASURE_WITH_UNIT (LENGTH_MEASURE( 1.000000000000000082E-05 ), #8779, 'distance_accuracy_value', 'NONE');
#3257 = CARTESIAN_POINT ( 'NONE',  ( 0.7499999999999991118, -14.29903810567666333, -0.5833333333333332593 ) ) ;
#3258 = ORIENTED_EDGE ( 'NONE', *, *, #3755, .F. ) ;
#3259 = ADVANCED_FACE ( 'NONE', ( #3830 ), #10480, .F. ) ;
#3260 =( BOUNDED_CURVE ( )  B_SPLINE_CURVE ( 2, ( #7762, #8767, #1506, #7867, #5419, #9464, #10426 ),
 .UNSPECIFIED., .F., .T. ) 
 B_SPLINE_CURVE_WITH_KNOTS ( ( 3, 2, 2, 3 ),
 ( 0.7500000000000000000, 0.7777777777777777901, 0.8055555555555554692, 0.8333333333333332593 ),
 .UNSPECIFIED. ) 
 CURVE ( )  GEOMETRIC_REPRESENTATION_ITEM ( )  RATIONAL_B_SPLINE_CURVE ( ( 1.000000000000000000, 0.8660254037844387076, 1.000000000000000000, 0.8660254037844387076, 1.000000000000000000, 0.8660254037844392627, 0.9999999999999994449 ) ) 
 REPRESENTATION_ITEM ( '' )  );
#3261 = EDGE_CURVE ( 'NONE', #1356, #9713, #10422, .T. ) ;
#3262 = EDGE_LOOP ( 'NONE', ( #4954, #10176, #7125, #4590 ) ) ;
#3263 = DIRECTION ( 'NONE',  ( -1.000000000000000000, -0.000000000000000000, -0.000000000000000000 ) ) ;
#3264 = CARTESIAN_POINT ( 'NONE',  ( -10.00000000000000000, 0.000000000000000000, 0.000000000000000000 ) ) ;
#3265 = ORIENTED_EDGE ( 'NONE', *, *, #1899, .T. ) ;
#3266 = CARTESIAN_POINT ( 'NONE',  ( -3.181980515339458027, -3.181980515339470905, 1.399999999999999689 ) ) ;
#3267 =( NAMED_UNIT ( * ) PLANE_ANGLE_UNIT ( ) SI_UNIT ( $, .RADIAN. ) );
#3268 = EDGE_LOOP ( 'NONE', ( #2202, #3538, #9592, #3952 ) ) ;
#3269 = CARTESIAN_POINT ( 'NONE',  ( -5.418398423912711870, -0.9480714621563917088, 11.07605171672202182 ) ) ;
#3270 = PRODUCT ( 'pin', 'pin', '', ( #8078 ) ) ;
#3271 = ORIENTED_EDGE ( 'NONE', *, *, #4674, .T. ) ;
#3272 = EDGE_CURVE ( 'NONE', #5618, #837, #7817, .T. ) ;
#3273 = EDGE_LOOP ( 'NONE', ( #3372, #9099, #9711, #958 ) ) ;
#3274 = VECTOR ( 'NONE', #756, 1000.000000000000000 ) ;
#3275 = PLANE ( 'NONE',  #10262 ) ;
#3276 = CARTESIAN_POINT ( 'NONE',  ( -2.000000000000024425, 15.00000000000000355, 5.999999999999987566 ) ) ;
#3277 = VERTEX_POINT ( 'NONE', #3938 ) ;
#3278 = CARTESIAN_POINT ( 'NONE',  ( 4.089228379062037178, -4.089228379062022967, 0.6999999999999997335 ) ) ;
#3279 = LINE ( 'NONE', #2273, #417 ) ;
#3280 = CARTESIAN_POINT ( 'NONE',  ( -5.432285873273256627, -0.8603895577212797852, 1.679999999999999938 ) ) ;
#3281 = VERTEX_POINT ( 'NONE', #5626 ) ;
#3282 = CARTESIAN_POINT ( 'NONE',  ( 1.500000000000000000, -13.86602540378444459, -0.6041666680322602678 ) ) ;
#3283 = AXIS2_PLACEMENT_3D ( 'NONE', #9724, #6630, #9882 ) ;
#3284 = ORIENTED_EDGE ( 'NONE', *, *, #7190, .T. ) ;
#3285 = CARTESIAN_POINT ( 'NONE',  ( -3.181725716174720991E-16, -14.73205080756888563, -2.624999999999999556 ) ) ;
#3286 = CARTESIAN_POINT ( 'NONE',  ( 1.999999999999986233, 15.00000000000000355, -4.000000000000009770 ) ) ;
#3287 = DIRECTION ( 'NONE',  ( 0.000000000000000000, 0.000000000000000000, 1.000000000000000000 ) ) ;
#3288 = CARTESIAN_POINT ( 'NONE',  ( 10.00000000000000000, 0.000000000000000000, 0.000000000000000000 ) ) ;
#3289 = LINE ( 'NONE', #8072, #2359 ) ;
#3290 = CARTESIAN_POINT ( 'NONE',  ( 4.258245684917310037, 2.064922774268912686, -0.8560517167220232926 ) ) ;
#3291 = ORIENTED_EDGE ( 'NONE', *, *, #3658, .T. ) ;
#3292 = CARTESIAN_POINT ( 'NONE',  ( 8.692241771943169307E-17, -11.58044919106553294, -0.2187500006827968746 ) ) ;
#3293 = CARTESIAN_POINT ( 'NONE',  ( 5.152728359536493663, 2.625446233515533745, 8.539999999999999147 ) ) ;
#3294 = DIRECTION ( 'NONE',  ( 1.000000000000000000, 0.000000000000000000, 0.000000000000000000 ) ) ;
#3295 = ITEM_DEFINED_TRANSFORMATION ( 'NONE', 'NONE', #7708,  #2101 ) ;
#3296 = CARTESIAN_POINT ( 'NONE',  ( 3.181980515339458471, 3.181980515339470461, 3.651811961182260059E-17 ) ) ;
#3297 = APPLICATION_CONTEXT ( 'automotive_design' ) ;
#3298 = CARTESIAN_POINT ( 'NONE',  ( 0.000000000000000000, -1.478016689125442706, 1.843143693225357538E-15 ) ) ;
#3299 = FACE_OUTER_BOUND ( 'NONE', #3770, .T. ) ;
#3300 = CARTESIAN_POINT ( 'NONE',  ( -2.625446233515515981, -5.152728359536500768, 1.259999999999999787 ) ) ;
#3301 = DIRECTION ( 'NONE',  ( -1.000000000000000000, 0.000000000000000000, -0.000000000000000000 ) ) ;
#3302 = DIRECTION ( 'NONE',  ( 0.3420201433256627732, 0.9396926207859105373, 0.000000000000000000 ) ) ;
#3303 = CARTESIAN_POINT ( 'NONE',  ( 4.049832306626335310, -1.963858260114701215, 1.556051716722023581 ) ) ;
#3304 = DIRECTION ( 'NONE',  ( -1.000000000000000000, 0.000000000000000000, 0.000000000000000000 ) ) ;
#3305 = DIRECTION ( 'NONE',  ( -1.000000000000000000, -0.000000000000000000, -0.000000000000000000 ) ) ;
#3306 = VECTOR ( 'NONE', #7514, 1000.000000000000000 ) ;
#3307 = EDGE_CURVE ( 'NONE', #165, #2420, #9414, .T. ) ;
#3308 = CARTESIAN_POINT ( 'NONE',  ( 4.658724279160018966, -0.8323763977770426425, 2.223948283277975779 ) ) ;
#3309 = CARTESIAN_POINT ( 'NONE',  ( 1.229367062500000163, -13.00000000000000533, -2.718750000682796486 ) ) ;
#3310 = ORIENTED_EDGE ( 'NONE', *, *, #7726, .T. ) ;
#3311 = ORIENTED_EDGE ( 'NONE', *, *, #7459, .T. ) ;
#3312 = CARTESIAN_POINT ( 'NONE',  ( 20.11292429676619520, -10.00000000000000000, 0.000000000000000000 ) ) ;
#3313 = VECTOR ( 'NONE', #7916, 1000.000000000000000 ) ;
#3314 = CYLINDRICAL_SURFACE ( 'NONE', #9167, 3.000000000000000000 ) ;
#3315 = ORIENTED_EDGE ( 'NONE', *, *, #8174, .T. ) ;
#3316 = AXIS2_PLACEMENT_3D ( 'NONE', #5469, #1611, #6207 ) ;
#3317 = CARTESIAN_POINT ( 'NONE',  ( -4.009529358847660596, 2.042957248827953265, 1.959999999999999964 ) ) ;
#3318 = DIRECTION ( 'NONE',  ( 0.000000000000000000, 0.000000000000000000, -1.000000000000000000 ) ) ;
#3319 = ORIENTED_EDGE ( 'NONE', *, *, #8304, .T. ) ;
#3320 = ADVANCED_FACE ( 'NONE', ( #6259 ), #547, .F. ) ;
#3321 = ADVANCED_FACE ( 'NONE', ( #3774 ), #442, .F. ) ;
#3322 = CARTESIAN_POINT ( 'NONE',  ( 4.173491630687861331, 2.231261971483781359, 9.536051716722020899 ) ) ;
#3323 = CIRCLE ( 'NONE', #9249, 3.000000000000000000 ) ;
#3324 = VERTEX_POINT ( 'NONE', #3144 ) ;
#3325 = AXIS2_PLACEMENT_3D ( 'NONE', #3025, #1325, #537 ) ;
#3326 = EDGE_LOOP ( 'NONE', ( #3483, #1193, #5703, #1848 ) ) ;
#3327 = DIRECTION ( 'NONE',  ( 0.7043149233066460235, -0.7043149233066438031, 0.08877487040322794287 ) ) ;
#3328 = EDGE_LOOP ( 'NONE', ( #5899, #9960, #1043, #5486, #5114, #9946, #3009, #2531, #7366, #9869, #3753, #266, #1301, #8204, #5393, #4645, #8414, #7177, #995, #2271, #8736, #9385, #5336, #625, #2312, #1571, #3000, #7896, #4650, #7933, #8814, #7473, #10452, #5542, #3195, #186 ) ) ;
#3329 = CARTESIAN_POINT ( 'NONE',  ( -4.900535883036028828, 2.496947748567499126, 4.759999999999999787 ) ) ;
#3330 = CARTESIAN_POINT ( 'NONE',  ( -5.711843387010018702, 0.9046671180729746187, 1.819999999999999396 ) ) ;
#3331 = CARTESIAN_POINT ( 'NONE',  ( 3.889087296526005488, 3.889087296526018811, -3.866961113726609188E-17 ) ) ;
#3332 = ORIENTED_EDGE ( 'NONE', *, *, #6482, .F. ) ;
#3333 = EDGE_CURVE ( 'NONE', #2958, #3937, #7918, .T. ) ;
#3334 = CARTESIAN_POINT ( 'NONE',  ( -3.181725716174720498E-16, -14.73205080756888385, -0.1875000013655935549 ) ) ;
#3335 = VERTEX_POINT ( 'NONE', #6576 ) ;
#3336 = CARTESIAN_POINT ( 'NONE',  ( 0.000000000000000000, 6.000000000000000000, -12.00000000000000000 ) ) ;
#3337 = DIRECTION ( 'NONE',  ( 1.000000000000000000, -0.000000000000000000, -0.000000000000000000 ) ) ;
#3338 = DIRECTION ( 'NONE',  ( 1.000000000000000000, 0.000000000000000000, 0.000000000000000000 ) ) ;
#3339 = CARTESIAN_POINT ( 'NONE',  ( 30.00000000000001066, 0.000000000000000000, -1.599999999999986766 ) ) ;
#3340 = CARTESIAN_POINT ( 'NONE',  ( 8.692241771943170539E-17, -11.58044919106553650, -2.718750000682796042 ) ) ;
#3341 = CARTESIAN_POINT ( 'NONE',  ( 0.7039550926810297371, 4.444597532678122853, 13.71999999999999886 ) ) ;
#3342 = ORIENTED_EDGE ( 'NONE', *, *, #5687, .F. ) ;
#3343 = CARTESIAN_POINT ( 'NONE',  ( 22.43558391966725907, -7.750000000000000000, -12.00000000000000000 ) ) ;
#3344 = CARTESIAN_POINT ( 'NONE',  ( 2.496947748567516889, -4.900535883036019946, 9.240000000000000213 ) ) ;
#3345 = PRODUCT_DEFINITION ( 'UNKNOWN', '', #7192, #80 ) ;
#3346 = DIRECTION ( 'NONE',  ( 1.000000000000000000, 0.000000000000000000, 0.000000000000000000 ) ) ;
#3347 = ITEM_DEFINED_TRANSFORMATION ( 'NONE', 'NONE', #10088,  #2101 ) ;
#3348 = CARTESIAN_POINT ( 'NONE',  ( 3.889087296526005488, 3.889087296526018811, 11.19999999999999751 ) ) ;
#3349 = CARTESIAN_POINT ( 'NONE',  ( 1.499999999999999778, -13.86602540378444637, -1.604166668032260379 ) ) ;
#3350 = DIRECTION ( 'NONE',  ( 0.000000000000000000, 1.000000000000000000, 0.000000000000000000 ) ) ;
#3351 = CARTESIAN_POINT ( 'NONE',  ( 1.300000000000000044, 0.000000000000000000, 0.000000000000000000 ) ) ;
#3352 = CARTESIAN_POINT ( 'NONE',  ( 0.000000000000000000, -13.00000000000000533, -3.000000000000000000 ) ) ;
#3353 = CARTESIAN_POINT ( 'NONE',  ( 4.173491630687861331, 2.231261971483781359, 6.736051716722023741 ) ) ;
#3354 = CARTESIAN_POINT ( 'NONE',  ( 13.82973899676619745, 6.000000000000000000, -12.00000000000000000 ) ) ;
#3355 = CARTESIAN_POINT ( 'NONE',  ( -4.458484982038663169, -0.6162731882459353550, 6.283948283277974944 ) ) ;
#3356 = ADVANCED_FACE ( 'NONE', ( #2615 ), #3409, .F. ) ;
#3357 = CARTESIAN_POINT ( 'NONE',  ( 1.300000000000000044, 1.478016689125442484, -1.626303258728256651E-15 ) ) ;
#3358 = EDGE_LOOP ( 'NONE', ( #302, #8772 ) ) ;
#3359 = CARTESIAN_POINT ( 'NONE',  ( 2.576046737280769605, -4.860232935257343456, 7.436051716722023031 ) ) ;
#3360 = ORIENTED_EDGE ( 'NONE', *, *, #203, .F. ) ;
#3361 = LINE ( 'NONE', #8147, #7986 ) ;
#3362 = ADVANCED_FACE ( 'NONE', ( #4144 ), #8922, .T. ) ;
#3363 = DIRECTION ( 'NONE',  ( 0.000000000000000000, -1.000000000000000000, 0.000000000000000000 ) ) ;
#3364 = VERTEX_POINT ( 'NONE', #2461 ) ;
#3365 = CARTESIAN_POINT ( 'NONE',  ( 0.7039550926810297371, 4.444597532678122853, 5.319999999999999396 ) ) ;
#3366 = FACE_BOUND ( 'NONE', #1794, .T. ) ;
#3367 = EDGE_LOOP ( 'NONE', ( #2116, #1542, #4704, #757 ) ) ;
#3368 = VECTOR ( 'NONE', #3159, 1000.000000000000000 ) ;
#3369 = CARTESIAN_POINT ( 'NONE',  ( -2.064922774268895811, -4.258245684917318918, 7.856051716722022071 ) ) ;
#3370 = CARTESIAN_POINT ( 'NONE',  ( -3.181725716174720991E-16, -14.73205080756888563, -1.187500001365593638 ) ) ;
#3371 = ORIENTED_EDGE ( 'NONE', *, *, #6815, .F. ) ;
#3372 = ORIENTED_EDGE ( 'NONE', *, *, #7501, .T. ) ;
#3373 = EDGE_CURVE ( 'NONE', #6398, #6869, #2475, .T. ) ;
#3374 = LINE ( 'NONE', #4170, #3989 ) ;
#3375 = EDGE_CURVE ( 'NONE', #6225, #8892, #10460, .T. ) ;
#3376 = PRESENTATION_LAYER_ASSIGNMENT (  '', '', ( #664 ) ) ;
#3377 = CARTESIAN_POINT ( 'NONE',  ( -0.7499999999999997780, -11.70096189432334555, -0.3333333333333334814 ) ) ;
#3378 = VERTEX_POINT ( 'NONE', #7275 ) ;
#3379 = COLOUR_RGB ( '', 0.31764706, 0.68627451, 0.89019608) ;
#3380 = CARTESIAN_POINT ( 'NONE',  ( 5.711843387010018702, -0.9046671180729751738, 6.019999999999999574 ) ) ;
#3381 = CARTESIAN_POINT ( 'NONE',  ( 5.432285873273257515, 0.8603895577212793411, 5.879999999999999893 ) ) ;
#3382 = CARTESIAN_POINT ( 'NONE',  ( -5.446173322633801384, -0.7727076532861678615, 9.083948283277974767 ) ) ;
#3383 = ORIENTED_EDGE ( 'NONE', *, *, #9858, .F. ) ;
#3384 = VECTOR ( 'NONE', #331, 1000.000000000000000 ) ;
#3385 = CARTESIAN_POINT ( 'NONE',  ( 1.229367062500000385, -12.29022459553277002, -2.177083334016129523 ) ) ;
#3386 = VECTOR ( 'NONE', #5592, 1000.000000000000000 ) ;
#3387 = ORIENTED_EDGE ( 'NONE', *, *, #2650, .F. ) ;
#3388 = ADVANCED_FACE ( 'NONE', ( #5676 ), #5831, .T. ) ;
#3389 = FACE_OUTER_BOUND ( 'NONE', #2694, .T. ) ;
#3390 = CARTESIAN_POINT ( 'NONE',  ( 1.878224253233805818, -10.00000000000000000, 0.000000000000000000 ) ) ;
#3391 = FACE_OUTER_BOUND ( 'NONE', #3102, .T. ) ;
#3392 = VERTEX_POINT ( 'NONE', #4195 ) ;
#3393 = DIRECTION ( 'NONE',  ( 0.000000000000000000, 0.000000000000000000, -1.000000000000000000 ) ) ;
#3394 = PRESENTATION_LAYER_ASSIGNMENT (  '', '', ( #2040 ) ) ;
#3395 = CARTESIAN_POINT ( 'NONE',  ( -2.607672531582950546E-16, -14.41955080893447416, -1.468750000682796708 ) ) ;
#3396 = CARTESIAN_POINT ( 'NONE',  ( 4.673326407553653361, -0.7401821875142523544, 11.61999999999999922 ) ) ;
#3397 = ORIENTED_EDGE ( 'NONE', *, *, #4198, .F. ) ;
#3398 = VECTOR ( 'NONE', #10102, 1000.000000000000000 ) ;
#3399 = DIRECTION ( 'NONE',  ( 0.000000000000000000, -1.000000000000000000, 0.000000000000000000 ) ) ;
#3400 = EDGE_CURVE ( 'NONE', #3392, #10377, #7329, .T. ) ;
#3401 = CARTESIAN_POINT ( 'NONE',  ( -5.432285873273256627, -0.8603895577212797852, 7.279999999999999361 ) ) ;
#3402 = VECTOR ( 'NONE', #8117, 1000.000000000000000 ) ;
#3403 = FACE_BOUND ( 'NONE', #7993, .T. ) ;
#3404 = AXIS2_PLACEMENT_3D ( 'NONE', #599, #5364, #649 ) ;
#3405 = ADVANCED_FACE ( 'NONE', ( #1017 ), #4942, .T. ) ;
#3406 = CARTESIAN_POINT ( 'NONE',  ( 5.152728359536493663, 2.625446233515533745, 5.739999999999998437 ) ) ;
#3407 = AXIS2_PLACEMENT_3D ( 'NONE', #6423, #7435, #4999 ) ;
#3408 = CYLINDRICAL_SURFACE ( 'NONE', #951, 3.000000000000000000 ) ;
#3409 = PLANE ( 'NONE',  #3816 ) ;
#3410 = AXIS2_PLACEMENT_3D ( 'NONE', #7068, #1461, #1622 ) ;
#3411 = LINE ( 'NONE', #3560, #260 ) ;
#3412 = CARTESIAN_POINT ( 'NONE',  ( -4.049832306626335310, 1.963858260114700327, 5.756051716722022427 ) ) ;
#3413 = DIRECTION ( 'NONE',  ( -1.000000000000000000, -0.000000000000000000, -0.000000000000000000 ) ) ;
#3414 = CARTESIAN_POINT ( 'NONE',  ( -0.6479879772514802738, 4.687928535947285091, 4.183948283277976188 ) ) ;
#3415 = FACE_OUTER_BOUND ( 'NONE', #8098, .T. ) ;
#3416 = ORIENTED_EDGE ( 'NONE', *, *, #6140, .F. ) ;
#3417 = CARTESIAN_POINT ( 'NONE',  ( -5.418398423912711870, -0.9480714621563917088, 2.676051716722023244 ) ) ;
#3418 = DIRECTION ( 'NONE',  ( 0.000000000000000000, -1.000000000000000000, 1.320393690296331133E-15 ) ) ;
#3419 = CARTESIAN_POINT ( 'NONE',  ( -26.99999999999998934, -13.00000000000000533, 0.000000000000000000 ) ) ;
#3420 = EDGE_LOOP ( 'NONE', ( #5544, #3205, #3319, #6366 ) ) ;
#3421 = CARTESIAN_POINT ( 'NONE',  ( -4.444597532678119300, -0.7039550926810477227, 1.679999999999999938 ) ) ;
#3422 = FILL_AREA_STYLE_COLOUR ( '', #7101 ) ;
#3423 = ORIENTED_EDGE ( 'NONE', *, *, #4279, .T. ) ;
#3424 = CARTESIAN_POINT ( 'NONE',  ( 3.119207202478379681, 3.244753828200549695, 6.596051716722022285 ) ) ;
#3425 = LINE ( 'NONE', #6598, #4798 ) ;
#3426 = ADVANCED_FACE ( 'NONE', ( #3299 ), #9780, .T. ) ;
#3427 = EDGE_LOOP ( 'NONE', ( #9323, #8889 ) ) ;
#3428 = ORIENTED_EDGE ( 'NONE', *, *, #1991, .T. ) ;
#3429 = DIRECTION ( 'NONE',  ( 0.000000000000000000, -1.000000000000000000, 0.000000000000000000 ) ) ;
#3430 = CARTESIAN_POINT ( 'NONE',  ( 0.000000000000000000, -13.00000000000000533, -3.000000000000000000 ) ) ;
#3431 = ORIENTED_EDGE ( 'NONE', *, *, #874, .F. ) ;
#3432 = CARTESIAN_POINT ( 'NONE',  ( 0.9968613283357860011, -5.697241258616382531, 1.976051716722022844 ) ) ;
#3433 = CARTESIAN_POINT ( 'NONE',  ( -4.089228379062038066, 4.089228379062021190, 4.900000000000000355 ) ) ;
#3434 = CARTESIAN_POINT ( 'NONE',  ( 0.9046671180729951578, -5.711843387010016926, 3.779999999999998472 ) ) ;
#3435 = ORIENTED_EDGE ( 'NONE', *, *, #925, .T. ) ;
#3436 = CARTESIAN_POINT ( 'NONE',  ( 1.229367062500000163, -13.00000000000000533, -0.2187500006827964583 ) ) ;
#3437 = EDGE_CURVE ( 'NONE', #5860, #7564, #232, .T. ) ;
#3438 =( REPRESENTATION_RELATIONSHIP ('NONE','NONE', #5100, #9430 ) REPRESENTATION_RELATIONSHIP_WITH_TRANSFORMATION ( #2345 )SHAPE_REPRESENTATION_RELATIONSHIP( ) );
#3439 = AXIS2_PLACEMENT_3D ( 'NONE', #9383, #8585, #423 ) ;
#3440 = ORIENTED_EDGE ( 'NONE', *, *, #2877, .F. ) ;
#3441 = DIRECTION ( 'NONE',  ( 0.000000000000000000, 0.000000000000000000, 1.000000000000000000 ) ) ;
#3442 = LINE ( 'NONE', #6910, #3231 ) ;
#3443 = CARTESIAN_POINT ( 'NONE',  ( 1.999999999999984901, 35.00000000000000000, 4.000000000000008882 ) ) ;
#3444 = ORIENTED_EDGE ( 'NONE', *, *, #9791, .F. ) ;
#3445 = CARTESIAN_POINT ( 'NONE',  ( 3.181980515339458471, 3.181980515339470461, 13.99999999999999822 ) ) ;
#3446 = VECTOR ( 'NONE', #8797, 1000.000000000000000 ) ;
#3447 = CARTESIAN_POINT ( 'NONE',  ( -2.607672531582950546E-16, -14.41955080893447416, -1.968750000682796708 ) ) ;
#3448 = CARTESIAN_POINT ( 'NONE',  ( -0.6479879772514802738, 4.687928535947285091, 1.383948283277976365 ) ) ;
#3449 = ORIENTED_EDGE ( 'NONE', *, *, #8054, .T. ) ;
#3450 = DIRECTION ( 'NONE',  ( 0.000000000000000000, 0.000000000000000000, 1.000000000000000000 ) ) ;
#3451 = EDGE_CURVE ( 'NONE', #65, #165, #176, .T. ) ;
#3452 = ADVANCED_FACE ( 'NONE', ( #6680, #1717, #6633 ), #9939, .T. ) ;
#3453 = CARTESIAN_POINT ( 'NONE',  ( -5.152728359536494551, -2.625446233515535077, 4.339999999999999858 ) ) ;
#3454 = CARTESIAN_POINT ( 'NONE',  ( 5.999999999999999112, -27.00000000000000711, -17.00000000000000000 ) ) ;
#3455 = MECHANICAL_DESIGN_GEOMETRIC_PRESENTATION_REPRESENTATION (  '', ( #7856 ), #9558 ) ;
#3456 = CARTESIAN_POINT ( 'NONE',  ( -2.496947748567517333, 4.900535883036019058, 10.63999999999999879 ) ) ;
#3457 = CARTESIAN_POINT ( 'NONE',  ( -2.000000000000000000, 52.93638525830372998, 0.000000000000000000 ) ) ;
#3458 = CARTESIAN_POINT ( 'NONE',  ( -31.74999999999995737, 3.367778697655221012E-16, -2.750000000000000000 ) ) ;
#3459 = LINE ( 'NONE', #6682, #10425 ) ;
#3460 = CARTESIAN_POINT ( 'NONE',  ( -4.940838830814703542, 2.417848759854245078, 14.15605171672202012 ) ) ;
#3461 = CARTESIAN_POINT ( 'NONE',  ( -15.00000000000000000, 19.99999999999999645, -9.000000000000000000 ) ) ;
#3462 = CIRCLE ( 'NONE', #4276, 3.000000000000000000 ) ;
#3463 = EDGE_CURVE ( 'NONE', #3378, #5694, #8082, .T. ) ;
#3464 = CARTESIAN_POINT ( 'NONE',  ( 4.258245684917310037, 2.064922774268912686, 1.943948283277976419 ) ) ;
#3465 = CARTESIAN_POINT ( 'NONE',  ( 0.6146835312500001924, -11.93533689329915326, -2.635416667349463449 ) ) ;
#3466 = ORIENTED_EDGE ( 'NONE', *, *, #2185, .T. ) ;
#3467 = CARTESIAN_POINT ( 'NONE',  ( 4.940838830814703542, -2.417848759854246410, 4.356051716722023848 ) ) ;
#3468 = DIRECTION ( 'NONE',  ( -0.000000000000000000, 1.320393690296331133E-15, 1.000000000000000000 ) ) ;
#3469 = DIRECTION ( 'NONE',  ( 0.000000000000000000, 0.8660254037844379305, -0.5000000000000014433 ) ) ;
#3470 = ORIENTED_EDGE ( 'NONE', *, *, #2326, .F. ) ;
#3471 = AXIS2_PLACEMENT_3D ( 'NONE', #4975, #2599, #1058 ) ;
#3472 = CARTESIAN_POINT ( 'NONE',  ( 4.673326407553653361, -0.7401821875142525764, 6.019999999999999574 ) ) ;
#3473 = CARTESIAN_POINT ( 'NONE',  ( 10.00000000000000000, -7.009698679648282749, -0.7308381473897593850 ) ) ;
#3474 = ORIENTED_EDGE ( 'NONE', *, *, #4640, .F. ) ;
#3475 = CARTESIAN_POINT ( 'NONE',  ( 4.687928535947288644, -0.6479879772514620662, 9.816051716722022036 ) ) ;
#3476 = LINE ( 'NONE', #4212, #3950 ) ;
#3477 = VERTEX_POINT ( 'NONE', #4042 ) ;
#3478 = DIRECTION ( 'NONE',  ( 1.000000000000000000, 0.000000000000000000, 6.123233995736766036E-17 ) ) ;
#3479 = AXIS2_PLACEMENT_3D ( 'NONE', #9861, #205, #5696 ) ;
#3480 = ORIENTED_EDGE ( 'NONE', *, *, #7475, .F. ) ;
#3481 = DIRECTION ( 'NONE',  ( 0.000000000000000000, 0.000000000000000000, 1.000000000000000000 ) ) ;
#3482 = FACE_OUTER_BOUND ( 'NONE', #9007, .T. ) ;
#3483 = ORIENTED_EDGE ( 'NONE', *, *, #7262, .T. ) ;
#3484 = CARTESIAN_POINT ( 'NONE',  ( -5.726445515403654873, 0.8124729078101847746, 2.816051716722022924 ) ) ;
#3485 = CARTESIAN_POINT ( 'NONE',  ( 5.711843387010018702, -0.9046671180729751738, 0.4199999999999999289 ) ) ;
#3486 = EDGE_CURVE ( 'NONE', #409, #5519, #4096, .T. ) ;
#3487 = CARTESIAN_POINT ( 'NONE',  ( 5.432285873273257515, 0.8603895577212793411, 11.47999999999999865 ) ) ;
#3488 = ORIENTED_EDGE ( 'NONE', *, *, #10079, .F. ) ;
#3489 = VECTOR ( 'NONE', #3528, 1000.000000000000000 ) ;
#3490 = CARTESIAN_POINT ( 'NONE',  ( -0.6146835312500006365, -14.06466310670085562, 0.1145833326505365929 ) ) ;
#3491 = VECTOR ( 'NONE', #4346, 1000.000000000000000 ) ;
#3492 =( NAMED_UNIT ( * ) PLANE_ANGLE_UNIT ( ) SI_UNIT ( $, .RADIAN. ) );
#3493 = EDGE_LOOP ( 'NONE', ( #1572, #7339, #5159, #1833 ) ) ;
#3494 = CARTESIAN_POINT ( 'NONE',  ( 0.000000000000000000, -13.00000000000000533, -3.000000000000000000 ) ) ;
#3495 = DIRECTION ( 'NONE',  ( 0.000000000000000000, 0.000000000000000000, -1.000000000000000000 ) ) ;
#3496 = EDGE_LOOP ( 'NONE', ( #314, #2151, #5786, #2639 ) ) ;
#3497 = DIRECTION ( 'NONE',  ( -0.000000000000000000, -1.000000000000000000, -0.000000000000000000 ) ) ;
#3498 = EDGE_CURVE ( 'NONE', #4944, #371, #7380, .T. ) ;
#3499 = CARTESIAN_POINT ( 'NONE',  ( -1.229367062500000163, -13.70977540446723708, -0.5520833340161299674 ) ) ;
#3500 = CARTESIAN_POINT ( 'NONE',  ( -4.458484982038663169, -0.6162731882459353550, 9.083948283277974767 ) ) ;
#3501 = ORIENTED_EDGE ( 'NONE', *, *, #10055, .T. ) ;
#3502 = CARTESIAN_POINT ( 'NONE',  ( 13.01080596966725622, 3.750000000000000000, -12.00000000000000000 ) ) ;
#3503 = CARTESIAN_POINT ( 'NONE',  ( 8.152164709283445276, -10.02539999999999942, -12.00000000000000000 ) ) ;
#3504 = CARTESIAN_POINT ( 'NONE',  ( 0.7499999999999991118, -14.29903810567666333, 0.3541666653010728805 ) ) ;
#3505 = CARTESIAN_POINT ( 'NONE',  ( 5.432285873273257515, 0.8603895577212793411, 8.679999999999997939 ) ) ;
#3506 = FACE_OUTER_BOUND ( 'NONE', #4266, .T. ) ;
#3507 = EDGE_CURVE ( 'NONE', #4078, #2259, #1427, .T. ) ;
#3508 = FACE_OUTER_BOUND ( 'NONE', #10119, .T. ) ;
#3509 = EDGE_CURVE ( 'NONE', #9806, #8450, #8905, .T. ) ;
#3510 = CYLINDRICAL_SURFACE ( 'NONE', #8258, 1.249999999999993339 ) ;
#3511 = CARTESIAN_POINT ( 'NONE',  ( -0.6162731882459178134, -4.458484982038665834, 2.116051716722023190 ) ) ;
#3512 = CARTESIAN_POINT ( 'NONE',  ( -1.229367062500000385, -13.70977540446723886, -1.427083334016129745 ) ) ;
#3513 = CARTESIAN_POINT ( 'NONE',  ( 3.244753828200538148, 3.119207202478391672, 13.00394828327797470 ) ) ;
#3514 = CARTESIAN_POINT ( 'NONE',  ( 0.6146835312500001924, -11.93533689329915326, -2.135416667349463449 ) ) ;
#3515 = ORIENTED_EDGE ( 'NONE', *, *, #8588, .T. ) ;
#3516 = CARTESIAN_POINT ( 'NONE',  ( -3.826313983664925811, -3.951860609387098489, 7.996051716722022640 ) ) ;
#3517 = EDGE_CURVE ( 'NONE', #5332, #4686, #3710, .T. ) ;
#3518 = DIRECTION ( 'NONE',  ( -1.000000000000000000, -4.625929269271485914E-16, 0.000000000000000000 ) ) ;
#3519 = CARTESIAN_POINT ( 'NONE',  ( 9.869213319667256457, -7.750000000000000000, -12.00000000000000000 ) ) ;
#3520 = ORIENTED_EDGE ( 'NONE', *, *, #6284, .F. ) ;
#3521 = CARTESIAN_POINT ( 'NONE',  ( -3.181980515339458027, -3.181980515339470905, 9.799999999999998934 ) ) ;
#3522 = CARTESIAN_POINT ( 'NONE',  ( 4.049832306626335310, -1.963858260114701215, 7.156051716722023670 ) ) ;
#3523 = CARTESIAN_POINT ( 'NONE',  ( -2.607672531582950546E-16, -14.41955080893447416, -2.468750000682796486 ) ) ;
#3524 = ORIENTED_EDGE ( 'NONE', *, *, #4095, .F. ) ;
#3525 = CARTESIAN_POINT ( 'NONE',  ( 0.000000000000000000, -31.99999999999999289, -6.938893903907228378E-15 ) ) ;
#3526 = ORIENTED_EDGE ( 'NONE', *, *, #4408, .T. ) ;
#3527 = ADVANCED_FACE ( 'NONE', ( #9344 ), #10197, .T. ) ;
#3528 = DIRECTION ( 'NONE',  ( -1.000000000000000000, 0.000000000000000000, 0.000000000000000000 ) ) ;
#3529 = LINE ( 'NONE', #9756, #2711 ) ;
#3530 = ORIENTED_EDGE ( 'NONE', *, *, #8031, .F. ) ;
#3531 = CARTESIAN_POINT ( 'NONE',  ( 4.155232146225751322, -4.023224611898307934, 4.496051716722022640 ) ) ;
#3532 = AXIS2_PLACEMENT_3D ( 'NONE', #3817, #9507, #7046 ) ;
#3533 = CARTESIAN_POINT ( 'NONE',  ( 3.889087296526005488, 3.889087296526018811, -3.866961113726609188E-17 ) ) ;
#3534 = CARTESIAN_POINT ( 'NONE',  ( -5.152728359536494551, -2.625446233515535077, 12.73999999999999488 ) ) ;
#3535 = ORIENTED_EDGE ( 'NONE', *, *, #2362, .F. ) ;
#3536 = CARTESIAN_POINT ( 'NONE',  ( -0.6146835312499998594, -11.93533689329915326, -1.552083334016129967 ) ) ;
#3537 = CIRCLE ( 'NONE', #4894, 6.248999999999999666 ) ;
#3538 = ORIENTED_EDGE ( 'NONE', *, *, #10211, .T. ) ;
#3539 = DIRECTION ( 'NONE',  ( 0.000000000000000000, 0.000000000000000000, 1.000000000000000000 ) ) ;
#3540 = VECTOR ( 'NONE', #9439, 1000.000000000000000 ) ;
#3541 = CARTESIAN_POINT ( 'NONE',  ( -2.000000000000000000, -0.1221666339523208161, -6.247805719894685694 ) ) ;
#3542 = VERTEX_POINT ( 'NONE', #7699 ) ;
#3543 = CARTESIAN_POINT ( 'NONE',  ( -2.000000000000000000, 0.000000000000000000, 0.000000000000000000 ) ) ;
#3544 = AXIS2_PLACEMENT_3D ( 'NONE', #4196, #2768, #8345 ) ;
#3545 = CARTESIAN_POINT ( 'NONE',  ( 1.500000000000000222, -13.00000000000000533, -2.562500001365593416 ) ) ;
#3546 = CARTESIAN_POINT ( 'NONE',  ( 8.692241771943170539E-17, -11.58044919106553650, -0.2187500006827969301 ) ) ;
#3547 = EDGE_CURVE ( 'NONE', #6004, #6822, #2131, .T. ) ;
#3548 = CARTESIAN_POINT ( 'NONE',  ( 3.244753828200538148, 3.119207202478391672, 13.00394828327797470 ) ) ;
#3549 = ORIENTED_EDGE ( 'NONE', *, *, #5389, .T. ) ;
#3550 = AXIS2_PLACEMENT_3D ( 'NONE', #2697, #9817, #4183 ) ;
#3551 = FACE_OUTER_BOUND ( 'NONE', #4073, .T. ) ;
#3552 = VECTOR ( 'NONE', #2315, 1000.000000000000000 ) ;
#3553 = CARTESIAN_POINT ( 'NONE',  ( -5.711843387010018702, 0.9046671180729746187, 13.01999999999999424 ) ) ;
#3554 = CARTESIAN_POINT ( 'NONE',  ( 1.500000000000000222, -13.00000000000000533, 0.4374999986344065284 ) ) ;
#3555 = EDGE_CURVE ( 'NONE', #1356, #3874, #6890, .T. ) ;
#3556 = CARTESIAN_POINT ( 'NONE',  ( 4.900535883036028828, -2.496947748567499126, 6.159999999999999254 ) ) ;
#3557 = VECTOR ( 'NONE', #7890, 1000.000000000000000 ) ;
#3558 = DIRECTION ( 'NONE',  ( -1.000000000000000000, 0.000000000000000000, 0.000000000000000000 ) ) ;
#3559 = DIRECTION ( 'NONE',  ( 0.000000000000000000, 0.000000000000000000, 1.000000000000000000 ) ) ;
#3560 = CARTESIAN_POINT ( 'NONE',  ( -1.500000000000000222, -13.00000000000000533, -3.000000000000000000 ) ) ;
#3561 = CARTESIAN_POINT ( 'NONE',  ( -2.042957248827969252, 4.009529358847651714, 2.239999999999999769 ) ) ;
#3562 = CARTESIAN_POINT ( 'NONE',  ( -1.229367062500000163, -13.00000000000000533, -0.9687500006827964860 ) ) ;
#3563 = AXIS2_PLACEMENT_3D ( 'NONE', #9835, #373, #7576 ) ;
#3564 = CARTESIAN_POINT ( 'NONE',  ( 1.963858260114715870, -4.049832306626327316, 11.04394828327797562 ) ) ;
#3565 = CARTESIAN_POINT ( 'NONE',  ( -0.6146835312499998594, -11.93533689329915326, -0.5520833340161299674 ) ) ;
#3567 = ORIENTED_EDGE ( 'NONE', *, *, #1681, .T. ) ;
#3566 =( GEOMETRIC_REPRESENTATION_CONTEXT ( 3 ) GLOBAL_UNCERTAINTY_ASSIGNED_CONTEXT ( ( #1455 ) ) GLOBAL_UNIT_ASSIGNED_CONTEXT ( ( #7334, #2354, #1565 ) ) REPRESENTATION_CONTEXT ( 'NONE', 'WORKASPACE' ) );
#3568 = CARTESIAN_POINT ( 'NONE',  ( -2.576046737280769605, 4.860232935257343456, 8.836051716722023386 ) ) ;
#3569 = VECTOR ( 'NONE', #37, 1000.000000000000000 ) ;
#3570 = DIRECTION ( 'NONE',  ( -1.000000000000000000, -0.000000000000000000, -0.000000000000000000 ) ) ;
#3571 = VECTOR ( 'NONE', #917, 1000.000000000000000 ) ;
#3572 = DIRECTION ( 'NONE',  ( 0.000000000000000000, -7.228014483236698281E-18, -1.000000000000000000 ) ) ;
#3573 = ORIENTED_EDGE ( 'NONE', *, *, #470, .F. ) ;
#3574 = CARTESIAN_POINT ( 'NONE',  ( 0.7039550926810297371, 4.444597532678122853, 8.119999999999999218 ) ) ;
#3575 = CIRCLE ( 'NONE', #7472, 2.000000000000003553 ) ;
#3576 = CARTESIAN_POINT ( 'NONE',  ( -0.7039550926810301812, -4.444597532678121965, 3.919999999999999929 ) ) ;
#3577 = EDGE_CURVE ( 'NONE', #4528, #9680, #4318, .T. ) ;
#3578 = CARTESIAN_POINT ( 'NONE',  ( -1.229367062500000163, -12.29022459553277002, -1.635416667349463227 ) ) ;
#3579 = ADVANCED_FACE ( 'NONE', ( #5253 ), #1923, .T. ) ;
#3580 = ORIENTED_EDGE ( 'NONE', *, *, #6969, .F. ) ;
#3581 = DIRECTION ( 'NONE',  ( -0.000000000000000000, -0.000000000000000000, -1.000000000000000000 ) ) ;
#3582 = VERTEX_POINT ( 'NONE', #2865 ) ;
#3583 = DIRECTION ( 'NONE',  ( 0.000000000000000000, 1.000000000000000000, 0.000000000000000000 ) ) ;
#3584 = CARTESIAN_POINT ( 'NONE',  ( 14.44459485323380754, 6.000000000000000000, -12.00000000000000000 ) ) ;
#3585 = EDGE_LOOP ( 'NONE', ( #6436, #7529, #2698, #2800 ) ) ;
#3586 = CARTESIAN_POINT ( 'NONE',  ( -0.8603895577212598011, -5.432285873273260179, 9.519999999999999574 ) ) ;
#3587 = CARTESIAN_POINT ( 'NONE',  ( -5.152728359536494551, -2.625446233515535077, 12.73999999999999488 ) ) ;
#3588 = CARTESIAN_POINT ( 'NONE',  ( -0.9046671180729963790, 5.711843387010016926, 13.57999999999999474 ) ) ;
#3589 = VERTEX_POINT ( 'NONE', #8495 ) ;
#3590 = CARTESIAN_POINT ( 'NONE',  ( -1.229367062500000163, -12.29022459553277002, -0.5104166673494631157 ) ) ;
#3591 = ADVANCED_FACE ( 'NONE', ( #8344 ), #1073, .T. ) ;
#3592 =( NAMED_UNIT ( * ) SI_UNIT ( $, .STERADIAN. ) SOLID_ANGLE_UNIT ( ) );
#3593 = VERTEX_POINT ( 'NONE', #2078 ) ;
#3594 = CARTESIAN_POINT ( 'NONE',  ( 27.00000000000001066, 0.000000000000000000, 0.000000000000000000 ) ) ;
#3595 = CARTESIAN_POINT ( 'NONE',  ( -31.74999999999995737, 0.000000000000000000, 0.000000000000000000 ) ) ;
#3596 = ORIENTED_EDGE ( 'NONE', *, *, #81, .F. ) ;
#3597 = LINE ( 'NONE', #1858, #1175 ) ;
#3598 = CARTESIAN_POINT ( 'NONE',  ( 1.070288219556879694, -11.94905607805280567, 1.518836458664385706E-16 ) ) ;
#3599 = CYLINDRICAL_SURFACE ( 'NONE', #657, 6.248999999999999666 ) ;
#3600 = CARTESIAN_POINT ( 'NONE',  ( 2.231261971483764484, 4.173491630687871101, 7.263948283277976259 ) ) ;
#3601 = ORIENTED_EDGE ( 'NONE', *, *, #8689, .F. ) ;
#3602 = DIRECTION ( 'NONE',  ( 0.3420201433256627732, 0.9396926207859105373, 0.000000000000000000 ) ) ;
#3603 = DIRECTION ( 'NONE',  ( 1.000000000000000000, 0.000000000000000000, 0.000000000000000000 ) ) ;
#3604 = DIRECTION ( 'NONE',  ( 1.000000000000000000, 0.000000000000000000, 0.000000000000000000 ) ) ;
#3605 = CYLINDRICAL_SURFACE ( 'NONE', #4142, 6.248999999999999666 ) ;
#3606 = PRODUCT_DEFINITION_SHAPE ( 'NONE', 'NONE',  #10510 ) ;
#3607 = VECTOR ( 'NONE', #8248, 1000.000000000000000 ) ;
#3608 = DIRECTION ( 'NONE',  ( 0.000000000000000000, 0.000000000000000000, 1.000000000000000000 ) ) ;
#3609 = DIRECTION ( 'NONE',  ( 0.000000000000000000, 0.000000000000000000, -1.000000000000000000 ) ) ;
#3610 = DIRECTION ( 'NONE',  ( -1.000000000000000000, 0.000000000000000000, -0.000000000000000000 ) ) ;
#3611 = CARTESIAN_POINT ( 'NONE',  ( 4.049832306626335310, -1.963858260114701215, 9.956051716722022604 ) ) ;
#3612 = CARTESIAN_POINT ( 'NONE',  ( 1.229367062500000385, -12.29022459553277002, -2.177083334016129523 ) ) ;
#3613 = CARTESIAN_POINT ( 'NONE',  ( 0.7916369971161419938, 4.430710083317576320, 12.72394828327797711 ) ) ;
#3614 = AXIS2_PLACEMENT_3D ( 'NONE', #5976, #2020, #8540 ) ;
#3615 = CARTESIAN_POINT ( 'NONE',  ( -1.229367062500000163, -12.29022459553277002, -2.010416667349463005 ) ) ;
#3616 = EDGE_LOOP ( 'NONE', ( #404, #1630, #6718, #4803 ) ) ;
#3617 = CARTESIAN_POINT ( 'NONE',  ( -10.00000000000000000, 0.000000000000000000, 0.000000000000000000 ) ) ;
#3618 = FACE_OUTER_BOUND ( 'NONE', #8196, .T. ) ;
#3619 = DIRECTION ( 'NONE',  ( 0.000000000000000000, 0.000000000000000000, -1.000000000000000000 ) ) ;
#3620 = ORIENTED_EDGE ( 'NONE', *, *, #1292, .T. ) ;
#3621 = CIRCLE ( 'NONE', #755, 0.5000000000000000000 ) ;
#3622 = EDGE_CURVE ( 'NONE', #9335, #201, #9238, .T. ) ;
#3623 = CARTESIAN_POINT ( 'NONE',  ( 4.009529358847659708, -2.042957248827953709, 8.959999999999999076 ) ) ;
#3624 =( LENGTH_UNIT ( ) NAMED_UNIT ( * ) SI_UNIT ( .MILLI., .METRE. ) );
#3625 = CARTESIAN_POINT ( 'NONE',  ( -4.215868657802586128, -2.148092372876348133, 4.339999999999999858 ) ) ;
#3626 = CARTESIAN_POINT ( 'NONE',  ( 1.500000000000000222, -13.00000000000000533, -3.000000000000000000 ) ) ;
#3627 = ORIENTED_EDGE ( 'NONE', *, *, #3901, .F. ) ;
#3628 =( NAMED_UNIT ( * ) SI_UNIT ( $, .STERADIAN. ) SOLID_ANGLE_UNIT ( ) );
#3629 = ORIENTED_EDGE ( 'NONE', *, *, #6933, .T. ) ;
#3630 = DIRECTION ( 'NONE',  ( 0.000000000000000000, 0.000000000000000000, -1.000000000000000000 ) ) ;
#3631 = CARTESIAN_POINT ( 'NONE',  ( -2.000000000000000000, -2.834406817834849601, -8.013497238472808704 ) ) ;
#3632 = VECTOR ( 'NONE', #4768, 1000.000000000000000 ) ;
#3633 = LINE ( 'NONE', #1352, #684 ) ;
#3634 = ORIENTED_EDGE ( 'NONE', *, *, #2488, .T. ) ;
#3635 = EDGE_CURVE ( 'NONE', #2207, #5532, #8442, .T. ) ;
#3636 = CARTESIAN_POINT ( 'NONE',  ( -5.711843387010018702, 0.9046671180729746187, 10.21999999999999709 ) ) ;
#3637 = ADVANCED_FACE ( 'NONE', ( #3508 ), #1279, .F. ) ;
#3638 = CARTESIAN_POINT ( 'NONE',  ( -2.625446233515515981, -5.152728359536500768, 12.45999999999999552 ) ) ;
#3639 = AXIS2_PLACEMENT_3D ( 'NONE', #3525, #5900, #2634 ) ;
#3640 = CARTESIAN_POINT ( 'NONE',  ( -3.889087296526005044, -3.889087296526019255, 6.999999999999999112 ) ) ;
#3641 = VERTEX_POINT ( 'NONE', #4505 ) ;
#3642 = DIRECTION ( 'NONE',  ( 0.000000000000000000, 0.000000000000000000, 1.000000000000000000 ) ) ;
#3643 = UNCERTAINTY_MEASURE_WITH_UNIT (LENGTH_MEASURE( 1.000000000000000082E-05 ), #1, 'distance_accuracy_value', 'NONE');
#3644 = VECTOR ( 'NONE', #2685, 1000.000000000000000 ) ;
#3645 = ORIENTED_EDGE ( 'NONE', *, *, #2088, .T. ) ;
#3646 = LINE ( 'NONE', #469, #6168 ) ;
#3647 = DIRECTION ( 'NONE',  ( 0.000000000000000000, -1.000000000000000000, -0.000000000000000000 ) ) ;
#3648 = EDGE_LOOP ( 'NONE', ( #2583, #3383, #4167, #544 ) ) ;
#3649 = EDGE_CURVE ( 'NONE', #2420, #8610, #4666, .T. ) ;
#3650 = DIRECTION ( 'NONE',  ( -1.000000000000000000, -0.000000000000000000, -0.000000000000000000 ) ) ;
#3651 = AXIS2_PLACEMENT_3D ( 'NONE', #1072, #2765, #381 ) ;
#3652 = DIRECTION ( 'NONE',  ( 0.000000000000000000, -1.000000000000000000, 1.026972870230479989E-15 ) ) ;
#3653 = DIRECTION ( 'NONE',  ( -0.000000000000000000, -0.000000000000000000, -1.000000000000000000 ) ) ;
#3654 = CARTESIAN_POINT ( 'NONE',  ( -3.244753828200538148, -3.119207202478392116, 11.60394828327797434 ) ) ;
#3655 = ORIENTED_EDGE ( 'NONE', *, *, #2171, .F. ) ;
#3656 = AXIS2_PLACEMENT_3D ( 'NONE', #2350, #6311, #10369 ) ;
#3657 = CARTESIAN_POINT ( 'NONE',  ( 16.15239861966725599, -7.750000000000000000, 0.000000000000000000 ) ) ;
#3658 = EDGE_CURVE ( 'NONE', #2344, #1777, #484, .T. ) ;
#3659 = DIRECTION ( 'NONE',  ( -1.000000000000000000, 0.000000000000000000, 0.000000000000000000 ) ) ;
#3660 = DIRECTION ( 'NONE',  ( 0.000000000000000000, 0.000000000000000000, 1.000000000000000000 ) ) ;
#3661 = LINE ( 'NONE', #6835, #7719 ) ;
#3662 = CARTESIAN_POINT ( 'NONE',  ( 0.000000000000000000, 0.000000000000000000, -14.00000000000000178 ) ) ;
#3663 = CYLINDRICAL_SURFACE ( 'NONE', #7081, 1.249999999999993339 ) ;
#3664 = CARTESIAN_POINT ( 'NONE',  ( 3.119207202478379681, 3.244753828200549695, 9.396051716722022107 ) ) ;
#3665 = CARTESIAN_POINT ( 'NONE',  ( -0.6146835312500006365, -14.06466310670085562, -1.885416667349463227 ) ) ;
#3666 = CARTESIAN_POINT ( 'NONE',  ( -5.697241258616385196, 0.9968613283357647958, 3.623948283277976135 ) ) ;
#3667 = DIRECTION ( 'NONE',  ( -0.9396926207859105373, 0.3420201433256627732, 0.000000000000000000 ) ) ;
#3668 = ORIENTED_EDGE ( 'NONE', *, *, #8731, .F. ) ;
#3669 = LINE ( 'NONE', #6897, #5923 ) ;
#3670 = CARTESIAN_POINT ( 'NONE',  ( 10.00000000000000178, 2.449293598294706414E-16, -2.000000000000000000 ) ) ;
#3671 = FACE_OUTER_BOUND ( 'NONE', #5284, .T. ) ;
#3672 = DIRECTION ( 'NONE',  ( -1.000000000000000000, 0.000000000000000000, -0.000000000000000000 ) ) ;
#3673 = EDGE_LOOP ( 'NONE', ( #8525, #6650, #8721, #4202 ) ) ;
#3674 =( BOUNDED_SURFACE ( )  B_SPLINE_SURFACE ( 3, 2, ( 
 ( #3533, #7566, #2592, #3485, #6758, #10020, #1796, #1742, #5024, #4322, #1950, #8268, #1098, #3330, #9005, #7517, #2689, #6708, #5173, #9966, #309, #2745, #151, #4969, #8214, #993, #5908, #5957, #9211, #5806, #9162, #4224, #7466, #8422, #209, #3433, #4121, #7360, #7409, #103, #6556, #1902, #3381, #5121, #948, #9808, #6608, #6656, #2537, #9913, #5756, #9058, #4174, #2642, #5858, #9110, #1846, #5069, #8322, #1051, #4272, #2898, #2003, #4480, #9371, #10069, #7729, #8523, #461, #5224, #1148, #2056, #5282, #6010, #6914, #1255, #2793, #4372, #8472, #411, #6812, #6867, #3688, #1204, #10170, #6119, #9263, #7618, #361, #3638, #10121, #3587, #6060, #4428, #7673, #2843, #9314, #7443, #4355, #9193, #342 ),
 ( #187, #6795, #9895, #1028, #8251, #977, #5105, #5154, #9139, #2672, #5940, #4203, #3417, #8352, #5205, #2775, #6640, #2624, #7498, #5840, #10051, #6691, #6586, #1081, #3467, #9999, #9844, #8451, #9947, #9092, #1827, #2572, #5887, #8299, #8404, #5050, #1182, #134, #4253, #1932, #5005, #1880, #1775, #7595, #4303, #241, #3359, #7550, #293, #9039, #3516, #6735, #2724, #1133, #5787, #5990, #3568, #9247, #1985, #4409, #8099, #3163, #7076, #10329, #1469, #6492, #3110, #4638, #620, #3904, #10388, #2370, #3269, #10497, #9752, #7884, #3848, #830, #4854, #4692, #7935, #5438, #3061, #4013, #6442, #6282, #8782, #2318, #7242, #9538, #4061, #5541, #3213, #1631, #4804, #8676, #1525, #43, #7296, #8728, #2264 ),
 ( #5595, #1412, #5489, #670, #7133, #6333, #8840, #4749, #9590, #7997, #9643, #2427, #726, #3957, #7187, #1582, #10444, #6388, #8049, #780, #9701, #5646, #8891, #198, #4211, #1087, #4311, #5849, #8205, #2679, #1734, #1787, #9100, #4113, #5112, #937, #7454, #9149, #4164, #8359, #3424, #7350, #93, #8995, #3522, #142, #1680, #8155, #7402, #3369, #9903, #300, #7507, #6745, #4907, #889, #7557, #1889, #4959, #6597, #2480, #3322, #1040, #3475, #6546, #5796, #9855, #4261, #9797, #5693, #2580, #248, #8937, #1834, #2526, #9049, #8257, #5745, #9956, #5894, #5014, #2631, #5060, #6647, #6699, #986, #8309, #10214, #1344, #5163, #9201, #400, #10159, #6110, #7822, #553, #2943, #1191, #6961, #8458, #1992 ),
 ( #3729, #8412, #3678, #3781, #6161, #1139, #4417, #2044, #9415, #1939, #5319, #9360, #10005, #4521, #350, #2885, #9254, #1295, #7604, #2735, #5998, #10109, #4362, #5272, #8563, #7659, #7765, #498, #3576, #2148, #2096, #3625, #2833, #5946, #6803, #4572, #6854, #5369, #10059, #2783, #8607, #5211, #6048, #9303, #8511, #1244, #4470, #7716, #451, #6905, #7922, #4624, #7870, #1508, #1568, #5530, #9577, #2356, #605, #3835, #4730, #1618, #9688, #10312, #7062, #3887, #3046, #3202, #3096, #2995, #7982, #10374, #6378, #6211, #4843, #6317, #6265, #9525, #9466, #2306, #4679, #4792, #2251, #8086, #7010, #5474, #5578, #1399, #8769, #8665, #4002, #715, #8713, #10265, #653, #3943, #5423, #7172, #1454, #10429, #7118 ),
 ( #3151, #6426, #9631, #2414, #8825, #8036, #767, #7231, #817, #10486, #2199, #5632, #8878, #8981, #974, #1876, #9089, #5101, #6478, #3255, #9944, #3464, #79, #3308, #8349, #9737, #2621, #5047, #4892, #7390, #922, #5837, #8927, #2668, #4151, #1823, #237, #3414, #4048, #7281, #2468, #5682, #5883, #6688, #6536, #9785, #30, #1666, #8295, #1021, #8142, #131, #3355, #4250, #877, #9135, #6582, #7495, #4103, #6637, #7336, #9840, #2569, #2515, #5728, #1724, #4948, #4200, #7436, #5001, #8192, #5784, #182, #9035, #1771, #8246, #9891, #1981, #1230, #7703, #9400, #2137, #4509, #2771, #8551, #10048, #3564, #6841, #4404, #2031, #4352, #5308, #9993, #5260, #5358, #1283, #2719, #5985, #3613, #7754, #3513 ),
 ( #8399, #9291, #6148, #3715, #7592, #1928, #8448, #335, #488, #7650, #7546, #8499, #388, #440, #290, #1077, #10098, #6792, #1130, #6730, #2824, #9243, #6098, #5202, #4299, #5937, #9189, #6894, #5150, #6037, #1177, #6949, #4456, #3666, #10147, #2872, #9348, #2082, #10203, #2929, #7103, #10302, #8598, #8021, #1556, #7049, #4715, #2342, #10250, #1387, #3872, #6251, #8810, #6412, #2240, #5565, #7809, #2983, #1494, #7157, #702, #9670, #7965, #4778, #3190, #6304, #10361, #7218, #10474, #3930, #3821, #754, #7855, #7909, #10414, #6202, #3987, #3030, #3084, #2401, #9511, #1329, #9563, #9455, #2184, #4612, #4559, #5461, #542, #3768, #8701, #1439, #5516, #6997, #3135, #5408, #8653, #590, #4664, #640, #2292 ),
 ( #9618, #8754, #6364, #2504, #7424, #14, #1011, #5717, #169, #1813, #4986, #9932, #1710, #911, #3244, #2611, #5825, #6466, #2556, #5774, #6572, #4191, #9881, #9024, #9078, #7486, #807, #4830, #6519, #1759, #8233, #3453, #6675, #5038, #7324, #8285, #4091, #8127, #4137, #8966, #9825, #8918, #4241, #4037, #964, #5620, #226, #7267, #67, #8179, #8865, #8076, #3401, #6628, #1606, #9723, #2454, #5668, #1655, #4880, #9776, #3293, #4938, #861, #7376, #120, #3344, #2707, #6720, #8387, #478, #10087, #2761, #5088, #1119, #6831, #10138, #7581, #1865, #8438, #2814, #4342, #1918, #5140, #9281, #1165, #378, #9982, #4393, #325, #2659, #2073, #6084, #3553, #2019, #6885, #4290, #5926, #7639, #6779, #2861 ) ),
 .UNSPECIFIED., .T., .F., .F. ) 
 B_SPLINE_SURFACE_WITH_KNOTS ( ( 4, 3, 4 ),
 ( 3, 2, 2, 2, 2, 2, 2, 2, 2, 2, 2, 2, 2, 2, 2, 2, 2, 2, 2, 2, 2, 2, 2, 2, 2, 2, 2, 2, 2, 2, 2, 2, 2, 2, 2, 2, 2, 2, 2, 2, 2, 2, 2, 2, 2, 2, 2, 2, 2, 2, 3 ),
 ( 0.000000000000000000, 0.5000000000000000000, 1.000000000000000000 ),
 ( 0.000000000000000000, 0.02000000000000000042, 0.04000000000000000083, 0.05999999999999999778, 0.08000000000000000167, 0.1000000000000000056, 0.1199999999999999956, 0.1400000000000000133, 0.1600000000000000033, 0.1799999999999999933, 0.2000000000000000111, 0.2200000000000000011, 0.2399999999999999911, 0.2600000000000000089, 0.2800000000000000266, 0.2999999999999999889, 0.3200000000000000067, 0.3400000000000000244, 0.3599999999999999867, 0.3800000000000000044, 0.4000000000000000222, 0.4199999999999999845, 0.4400000000000000022, 0.4600000000000000200, 0.4799999999999999822, 0.5000000000000000000, 0.5200000000000000178, 0.5400000000000000355, 0.5600000000000000533, 0.5799999999999999600, 0.5999999999999999778, 0.6199999999999999956, 0.6400000000000000133, 0.6600000000000000311, 0.6800000000000000488, 0.6999999999999999556, 0.7199999999999999734, 0.7399999999999999911, 0.7600000000000000089, 0.7800000000000000266, 0.8000000000000000444, 0.8199999999999999512, 0.8399999999999999689, 0.8599999999999999867, 0.8800000000000000044, 0.9000000000000000222, 0.9200000000000000400, 0.9399999999999999467, 0.9599999999999999645, 0.9799999999999999822, 1.000000000000000000 ),
 .UNSPECIFIED. ) 
 GEOMETRIC_REPRESENTATION_ITEM ( )  RATIONAL_B_SPLINE_SURFACE ( (
 ( 1.000000000000000000, 0.9510565162951535312, 1.000000000000000000, 0.9510565162951535312, 1.000000000000000000, 0.9510565162951535312, 1.000000000000000000, 0.9510565162951535312, 1.000000000000000000, 0.9510565162951535312, 1.000000000000000000, 0.9510565162951535312, 1.000000000000000000, 0.9510565162951535312, 1.000000000000000000, 0.9510565162951535312, 1.000000000000000000, 0.9510565162951535312, 1.000000000000000000, 0.9510565162951535312, 1.000000000000000000, 0.9510565162951535312, 1.000000000000000000, 0.9510565162951535312, 1.000000000000000000, 0.9510565162951535312, 1.000000000000000000, 0.9510565162951535312, 1.000000000000000000, 0.9510565162951535312, 1.000000000000000000, 0.9510565162951535312, 1.000000000000000000, 0.9510565162951535312, 1.000000000000000000, 0.9510565162951535312, 1.000000000000000000, 0.9510565162951535312, 1.000000000000000000, 0.9510565162951535312, 1.000000000000000000, 0.9510565162951535312, 1.000000000000000000, 0.9510565162951535312, 1.000000000000000000, 0.9510565162951535312, 1.000000000000000000, 0.9510565162951535312, 1.000000000000000000, 0.9510565162951535312, 1.000000000000000000, 0.9510565162951535312, 1.000000000000000000, 0.9510565162951535312, 1.000000000000000000, 0.9510565162951535312, 1.000000000000000000, 0.9510565162951535312, 1.000000000000000000, 0.9510565162951535312, 1.000000000000000000, 0.9510565162951535312, 1.000000000000000000, 0.9510565162951535312, 1.000000000000000000, 0.9510565162951535312, 1.000000000000000000, 0.9510565162951535312, 1.000000000000000000, 0.9510565162951535312, 1.000000000000000000, 0.9510565162951535312, 1.000000000000000000, 0.9510565162951535312, 1.000000000000000000, 0.9510565162951535312, 1.000000000000000000, 0.9510565162951535312, 1.000000000000000000, 0.9510565162951535312, 1.000000000000000000, 0.9510565162951535312, 1.000000000000000000, 0.9510565162951535312, 1.000000000000000000, 0.9510565162951535312, 1.000000000000000000, 0.9510565162951535312, 1.000000000000000000, 0.9510565162951535312, 1.000000000000000000, 0.9510565162951535312, 1.000000000000000000, 0.9510565162951535312, 1.000000000000000000, 0.9510565162951535312, 1.000000000000000000, 0.9510565162951535312, 1.000000000000000000, 0.9510565162951535312, 1.000000000000000000),
 ( 0.3333333333333333703, 0.3170188387650512141, 0.3333333333333333703, 0.3170188387650512141, 0.3333333333333333703, 0.3170188387650512141, 0.3333333333333333703, 0.3170188387650512141, 0.3333333333333333703, 0.3170188387650512141, 0.3333333333333333703, 0.3170188387650512141, 0.3333333333333333703, 0.3170188387650512141, 0.3333333333333333703, 0.3170188387650512141, 0.3333333333333333703, 0.3170188387650512141, 0.3333333333333333703, 0.3170188387650512141, 0.3333333333333333703, 0.3170188387650512141, 0.3333333333333333703, 0.3170188387650512141, 0.3333333333333333703, 0.3170188387650512141, 0.3333333333333333703, 0.3170188387650512141, 0.3333333333333333703, 0.3170188387650512141, 0.3333333333333333703, 0.3170188387650512141, 0.3333333333333333703, 0.3170188387650512141, 0.3333333333333333703, 0.3170188387650512141, 0.3333333333333333703, 0.3170188387650512141, 0.3333333333333333703, 0.3170188387650512141, 0.3333333333333333703, 0.3170188387650512141, 0.3333333333333333703, 0.3170188387650512141, 0.3333333333333333703, 0.3170188387650512141, 0.3333333333333333703, 0.3170188387650512141, 0.3333333333333333703, 0.3170188387650512141, 0.3333333333333333703, 0.3170188387650512141, 0.3333333333333333703, 0.3170188387650512141, 0.3333333333333333703, 0.3170188387650512141, 0.3333333333333333703, 0.3170188387650512141, 0.3333333333333333703, 0.3170188387650512141, 0.3333333333333333703, 0.3170188387650512141, 0.3333333333333333703, 0.3170188387650512141, 0.3333333333333333703, 0.3170188387650512141, 0.3333333333333333703, 0.3170188387650512141, 0.3333333333333333703, 0.3170188387650512141, 0.3333333333333333703, 0.3170188387650512141, 0.3333333333333333703, 0.3170188387650512141, 0.3333333333333333703, 0.3170188387650512141, 0.3333333333333333703, 0.3170188387650512141, 0.3333333333333333703, 0.3170188387650512141, 0.3333333333333333703, 0.3170188387650512141, 0.3333333333333333703, 0.3170188387650512141, 0.3333333333333333703, 0.3170188387650512141, 0.3333333333333333703, 0.3170188387650512141, 0.3333333333333333703, 0.3170188387650512141, 0.3333333333333333703, 0.3170188387650512141, 0.3333333333333333703, 0.3170188387650512141, 0.3333333333333333703, 0.3170188387650512141, 0.3333333333333333703, 0.3170188387650512141, 0.3333333333333333703, 0.3170188387650512141, 0.3333333333333333703),
 ( 0.3333333333333333703, 0.3170188387650512141, 0.3333333333333333703, 0.3170188387650512141, 0.3333333333333333703, 0.3170188387650512141, 0.3333333333333333703, 0.3170188387650512141, 0.3333333333333333703, 0.3170188387650512141, 0.3333333333333333703, 0.3170188387650512141, 0.3333333333333333703, 0.3170188387650512141, 0.3333333333333333703, 0.3170188387650512141, 0.3333333333333333703, 0.3170188387650512141, 0.3333333333333333703, 0.3170188387650512141, 0.3333333333333333703, 0.3170188387650512141, 0.3333333333333333703, 0.3170188387650512141, 0.3333333333333333703, 0.3170188387650512141, 0.3333333333333333703, 0.3170188387650512141, 0.3333333333333333703, 0.3170188387650512141, 0.3333333333333333703, 0.3170188387650512141, 0.3333333333333333703, 0.3170188387650512141, 0.3333333333333333703, 0.3170188387650512141, 0.3333333333333333703, 0.3170188387650512141, 0.3333333333333333703, 0.3170188387650512141, 0.3333333333333333703, 0.3170188387650512141, 0.3333333333333333703, 0.3170188387650512141, 0.3333333333333333703, 0.3170188387650512141, 0.3333333333333333703, 0.3170188387650512141, 0.3333333333333333703, 0.3170188387650512141, 0.3333333333333333703, 0.3170188387650512141, 0.3333333333333333703, 0.3170188387650512141, 0.3333333333333333703, 0.3170188387650512141, 0.3333333333333333703, 0.3170188387650512141, 0.3333333333333333703, 0.3170188387650512141, 0.3333333333333333703, 0.3170188387650512141, 0.3333333333333333703, 0.3170188387650512141, 0.3333333333333333703, 0.3170188387650512141, 0.3333333333333333703, 0.3170188387650512141, 0.3333333333333333703, 0.3170188387650512141, 0.3333333333333333703, 0.3170188387650512141, 0.3333333333333333703, 0.3170188387650512141, 0.3333333333333333703, 0.3170188387650512141, 0.3333333333333333703, 0.3170188387650512141, 0.3333333333333333703, 0.3170188387650512141, 0.3333333333333333703, 0.3170188387650512141, 0.3333333333333333703, 0.3170188387650512141, 0.3333333333333333703, 0.3170188387650512141, 0.3333333333333333703, 0.3170188387650512141, 0.3333333333333333703, 0.3170188387650512141, 0.3333333333333333703, 0.3170188387650512141, 0.3333333333333333703, 0.3170188387650512141, 0.3333333333333333703, 0.3170188387650512141, 0.3333333333333333703, 0.3170188387650512141, 0.3333333333333333703, 0.3170188387650512141, 0.3333333333333333703),
 ( 1.000000000000000000, 0.9510565162951535312, 1.000000000000000000, 0.9510565162951535312, 1.000000000000000000, 0.9510565162951535312, 1.000000000000000000, 0.9510565162951535312, 1.000000000000000000, 0.9510565162951535312, 1.000000000000000000, 0.9510565162951535312, 1.000000000000000000, 0.9510565162951535312, 1.000000000000000000, 0.9510565162951535312, 1.000000000000000000, 0.9510565162951535312, 1.000000000000000000, 0.9510565162951535312, 1.000000000000000000, 0.9510565162951535312, 1.000000000000000000, 0.9510565162951535312, 1.000000000000000000, 0.9510565162951535312, 1.000000000000000000, 0.9510565162951535312, 1.000000000000000000, 0.9510565162951535312, 1.000000000000000000, 0.9510565162951535312, 1.000000000000000000, 0.9510565162951535312, 1.000000000000000000, 0.9510565162951535312, 1.000000000000000000, 0.9510565162951535312, 1.000000000000000000, 0.9510565162951535312, 1.000000000000000000, 0.9510565162951535312, 1.000000000000000000, 0.9510565162951535312, 1.000000000000000000, 0.9510565162951535312, 1.000000000000000000, 0.9510565162951535312, 1.000000000000000000, 0.9510565162951535312, 1.000000000000000000, 0.9510565162951535312, 1.000000000000000000, 0.9510565162951535312, 1.000000000000000000, 0.9510565162951535312, 1.000000000000000000, 0.9510565162951535312, 1.000000000000000000, 0.9510565162951535312, 1.000000000000000000, 0.9510565162951535312, 1.000000000000000000, 0.9510565162951535312, 1.000000000000000000, 0.9510565162951535312, 1.000000000000000000, 0.9510565162951535312, 1.000000000000000000, 0.9510565162951535312, 1.000000000000000000, 0.9510565162951535312, 1.000000000000000000, 0.9510565162951535312, 1.000000000000000000, 0.9510565162951535312, 1.000000000000000000, 0.9510565162951535312, 1.000000000000000000, 0.9510565162951535312, 1.000000000000000000, 0.9510565162951535312, 1.000000000000000000, 0.9510565162951535312, 1.000000000000000000, 0.9510565162951535312, 1.000000000000000000, 0.9510565162951535312, 1.000000000000000000, 0.9510565162951535312, 1.000000000000000000, 0.9510565162951535312, 1.000000000000000000, 0.9510565162951535312, 1.000000000000000000, 0.9510565162951535312, 1.000000000000000000, 0.9510565162951535312, 1.000000000000000000, 0.9510565162951535312, 1.000000000000000000),
 ( 0.3333333333333333703, 0.3170188387650512141, 0.3333333333333333703, 0.3170188387650512141, 0.3333333333333333703, 0.3170188387650512141, 0.3333333333333333703, 0.3170188387650512141, 0.3333333333333333703, 0.3170188387650512141, 0.3333333333333333703, 0.3170188387650512141, 0.3333333333333333703, 0.3170188387650512141, 0.3333333333333333703, 0.3170188387650512141, 0.3333333333333333703, 0.3170188387650512141, 0.3333333333333333703, 0.3170188387650512141, 0.3333333333333333703, 0.3170188387650512141, 0.3333333333333333703, 0.3170188387650512141, 0.3333333333333333703, 0.3170188387650512141, 0.3333333333333333703, 0.3170188387650512141, 0.3333333333333333703, 0.3170188387650512141, 0.3333333333333333703, 0.3170188387650512141, 0.3333333333333333703, 0.3170188387650512141, 0.3333333333333333703, 0.3170188387650512141, 0.3333333333333333703, 0.3170188387650512141, 0.3333333333333333703, 0.3170188387650512141, 0.3333333333333333703, 0.3170188387650512141, 0.3333333333333333703, 0.3170188387650512141, 0.3333333333333333703, 0.3170188387650512141, 0.3333333333333333703, 0.3170188387650512141, 0.3333333333333333703, 0.3170188387650512141, 0.3333333333333333703, 0.3170188387650512141, 0.3333333333333333703, 0.3170188387650512141, 0.3333333333333333703, 0.3170188387650512141, 0.3333333333333333703, 0.3170188387650512141, 0.3333333333333333703, 0.3170188387650512141, 0.3333333333333333703, 0.3170188387650512141, 0.3333333333333333703, 0.3170188387650512141, 0.3333333333333333703, 0.3170188387650512141, 0.3333333333333333703, 0.3170188387650512141, 0.3333333333333333703, 0.3170188387650512141, 0.3333333333333333703, 0.3170188387650512141, 0.3333333333333333703, 0.3170188387650512141, 0.3333333333333333703, 0.3170188387650512141, 0.3333333333333333703, 0.3170188387650512141, 0.3333333333333333703, 0.3170188387650512141, 0.3333333333333333703, 0.3170188387650512141, 0.3333333333333333703, 0.3170188387650512141, 0.3333333333333333703, 0.3170188387650512141, 0.3333333333333333703, 0.3170188387650512141, 0.3333333333333333703, 0.3170188387650512141, 0.3333333333333333703, 0.3170188387650512141, 0.3333333333333333703, 0.3170188387650512141, 0.3333333333333333703, 0.3170188387650512141, 0.3333333333333333703, 0.3170188387650512141, 0.3333333333333333703, 0.3170188387650512141, 0.3333333333333333703),
 ( 0.3333333333333333703, 0.3170188387650512141, 0.3333333333333333703, 0.3170188387650512141, 0.3333333333333333703, 0.3170188387650512141, 0.3333333333333333703, 0.3170188387650512141, 0.3333333333333333703, 0.3170188387650512141, 0.3333333333333333703, 0.3170188387650512141, 0.3333333333333333703, 0.3170188387650512141, 0.3333333333333333703, 0.3170188387650512141, 0.3333333333333333703, 0.3170188387650512141, 0.3333333333333333703, 0.3170188387650512141, 0.3333333333333333703, 0.3170188387650512141, 0.3333333333333333703, 0.3170188387650512141, 0.3333333333333333703, 0.3170188387650512141, 0.3333333333333333703, 0.3170188387650512141, 0.3333333333333333703, 0.3170188387650512141, 0.3333333333333333703, 0.3170188387650512141, 0.3333333333333333703, 0.3170188387650512141, 0.3333333333333333703, 0.3170188387650512141, 0.3333333333333333703, 0.3170188387650512141, 0.3333333333333333703, 0.3170188387650512141, 0.3333333333333333703, 0.3170188387650512141, 0.3333333333333333703, 0.3170188387650512141, 0.3333333333333333703, 0.3170188387650512141, 0.3333333333333333703, 0.3170188387650512141, 0.3333333333333333703, 0.3170188387650512141, 0.3333333333333333703, 0.3170188387650512141, 0.3333333333333333703, 0.3170188387650512141, 0.3333333333333333703, 0.3170188387650512141, 0.3333333333333333703, 0.3170188387650512141, 0.3333333333333333703, 0.3170188387650512141, 0.3333333333333333703, 0.3170188387650512141, 0.3333333333333333703, 0.3170188387650512141, 0.3333333333333333703, 0.3170188387650512141, 0.3333333333333333703, 0.3170188387650512141, 0.3333333333333333703, 0.3170188387650512141, 0.3333333333333333703, 0.3170188387650512141, 0.3333333333333333703, 0.3170188387650512141, 0.3333333333333333703, 0.3170188387650512141, 0.3333333333333333703, 0.3170188387650512141, 0.3333333333333333703, 0.3170188387650512141, 0.3333333333333333703, 0.3170188387650512141, 0.3333333333333333703, 0.3170188387650512141, 0.3333333333333333703, 0.3170188387650512141, 0.3333333333333333703, 0.3170188387650512141, 0.3333333333333333703, 0.3170188387650512141, 0.3333333333333333703, 0.3170188387650512141, 0.3333333333333333703, 0.3170188387650512141, 0.3333333333333333703, 0.3170188387650512141, 0.3333333333333333703, 0.3170188387650512141, 0.3333333333333333703, 0.3170188387650512141, 0.3333333333333333703),
 ( 1.000000000000000000, 0.9510565162951535312, 1.000000000000000000, 0.9510565162951535312, 1.000000000000000000, 0.9510565162951535312, 1.000000000000000000, 0.9510565162951535312, 1.000000000000000000, 0.9510565162951535312, 1.000000000000000000, 0.9510565162951535312, 1.000000000000000000, 0.9510565162951535312, 1.000000000000000000, 0.9510565162951535312, 1.000000000000000000, 0.9510565162951535312, 1.000000000000000000, 0.9510565162951535312, 1.000000000000000000, 0.9510565162951535312, 1.000000000000000000, 0.9510565162951535312, 1.000000000000000000, 0.9510565162951535312, 1.000000000000000000, 0.9510565162951535312, 1.000000000000000000, 0.9510565162951535312, 1.000000000000000000, 0.9510565162951535312, 1.000000000000000000, 0.9510565162951535312, 1.000000000000000000, 0.9510565162951535312, 1.000000000000000000, 0.9510565162951535312, 1.000000000000000000, 0.9510565162951535312, 1.000000000000000000, 0.9510565162951535312, 1.000000000000000000, 0.9510565162951535312, 1.000000000000000000, 0.9510565162951535312, 1.000000000000000000, 0.9510565162951535312, 1.000000000000000000, 0.9510565162951535312, 1.000000000000000000, 0.9510565162951535312, 1.000000000000000000, 0.9510565162951535312, 1.000000000000000000, 0.9510565162951535312, 1.000000000000000000, 0.9510565162951535312, 1.000000000000000000, 0.9510565162951535312, 1.000000000000000000, 0.9510565162951535312, 1.000000000000000000, 0.9510565162951535312, 1.000000000000000000, 0.9510565162951535312, 1.000000000000000000, 0.9510565162951535312, 1.000000000000000000, 0.9510565162951535312, 1.000000000000000000, 0.9510565162951535312, 1.000000000000000000, 0.9510565162951535312, 1.000000000000000000, 0.9510565162951535312, 1.000000000000000000, 0.9510565162951535312, 1.000000000000000000, 0.9510565162951535312, 1.000000000000000000, 0.9510565162951535312, 1.000000000000000000, 0.9510565162951535312, 1.000000000000000000, 0.9510565162951535312, 1.000000000000000000, 0.9510565162951535312, 1.000000000000000000, 0.9510565162951535312, 1.000000000000000000, 0.9510565162951535312, 1.000000000000000000, 0.9510565162951535312, 1.000000000000000000, 0.9510565162951535312, 1.000000000000000000, 0.9510565162951535312, 1.000000000000000000, 0.9510565162951535312, 1.000000000000000000) ) ) 
 REPRESENTATION_ITEM ( '' )  SURFACE ( )  );
#3675 = CARTESIAN_POINT ( 'NONE',  ( -4.009529358847660596, 2.042957248827953265, 13.15999999999999837 ) ) ;
#3676 = EDGE_CURVE ( 'NONE', #2207, #3855, #8409, .T. ) ;
#3677 = LINE ( 'NONE', #4520, #7801 ) ;
#3678 = CARTESIAN_POINT ( 'NONE',  ( 4.444597532678119300, 0.7039550926810472786, 0.2799999999999999711 ) ) ;
#3679 = CARTESIAN_POINT ( 'NONE',  ( 1.060575238724907038E-16, -11.26794919243112680, -2.875000000000000000 ) ) ;
#3680 = ORIENTED_EDGE ( 'NONE', *, *, #3373, .F. ) ;
#3681 = ADVANCED_FACE ( 'NONE', ( #1226 ), #9394, .F. ) ;
#3682 = EDGE_LOOP ( 'NONE', ( #6964, #6760, #4126, #6389 ) ) ;
#3683 = CARTESIAN_POINT ( 'NONE',  ( 10.00000000000000000, 4.561279057474473930, -4.271385531633122845 ) ) ;
#3684 = CARTESIAN_POINT ( 'NONE',  ( 2.500000000000000000, 3.061616997868383141E-16, -4.000000000000000000 ) ) ;
#3685 = CARTESIAN_POINT ( 'NONE',  ( 10.00000000000000000, 0.000000000000000000, 0.000000000000000000 ) ) ;
#3686 = ORIENTED_EDGE ( 'NONE', *, *, #2759, .T. ) ;
#3687 = CARTESIAN_POINT ( 'NONE',  ( 5.110351332421769754, 2.708615832122969191, 9.536051716722020899 ) ) ;
#3688 = CARTESIAN_POINT ( 'NONE',  ( 5.432285873273257515, 0.8603895577212793411, 11.47999999999999865 ) ) ;
#3689 = CARTESIAN_POINT ( 'NONE',  ( -4.089228379062038066, 4.089228379062021190, 10.50000000000000000 ) ) ;
#3690 = VERTEX_POINT ( 'NONE', #2130 ) ;
#3691 = CYLINDRICAL_SURFACE ( 'NONE', #5930, 3.000000000000000000 ) ;
#3692 = ORIENTED_EDGE ( 'NONE', *, *, #7915, .F. ) ;
#3693 = VERTEX_POINT ( 'NONE', #6245 ) ;
#3694 = LINE ( 'NONE', #5385, #2968 ) ;
#3695 = LINE ( 'NONE', #9488, #5740 ) ;
#3696 = EDGE_LOOP ( 'NONE', ( #4496, #4897, #8364, #8835 ) ) ;
#3697 = CARTESIAN_POINT ( 'NONE',  ( 0.4444353696672553311, 3.750000000000000000, -12.00000000000000000 ) ) ;
#3698 = PLANE ( 'NONE',  #6668 ) ;
#3699 = CARTESIAN_POINT ( 'NONE',  ( -4.458484982038663169, -0.6162731882459353550, 11.88394828327797548 ) ) ;
#3700 = EDGE_LOOP ( 'NONE', ( #5410, #5213 ) ) ;
#3701 = CARTESIAN_POINT ( 'NONE',  ( -1.500000000000000000, -12.13397459621556607, -2.354166668032260379 ) ) ;
#3702 = VECTOR ( 'NONE', #7850, 1000.000000000000000 ) ;
#3703 = LINE ( 'NONE', #4500, #6300 ) ;
#3704 = EDGE_CURVE ( 'NONE', #247, #7195, #1548, .T. ) ;
#3705 = DIRECTION ( 'NONE',  ( 0.000000000000000000, -0.000000000000000000, 1.000000000000000000 ) ) ;
#3706 = ADVANCED_FACE ( 'NONE', ( #636, #8696 ), #7959, .T. ) ;
#3707 = DIRECTION ( 'NONE',  ( 0.000000000000000000, 0.000000000000000000, 1.000000000000000000 ) ) ;
#3708 = CARTESIAN_POINT ( 'NONE',  ( 8.152164709283445276, 6.025400000000000311, -12.00000000000000000 ) ) ;
#3709 = DIRECTION ( 'NONE',  ( 0.000000000000000000, 0.000000000000000000, -1.000000000000000000 ) ) ;
#3710 = LINE ( 'NONE', #436, #8732 ) ;
#3711 = CARTESIAN_POINT ( 'NONE',  ( 25.00000000000000000, 0.000000000000000000, -12.00000000000000000 ) ) ;
#3712 = CARTESIAN_POINT ( 'NONE',  ( 2.122056237541221524, -3.969226411068978777, 13.03605171672202090 ) ) ;
#3713 = AXIS2_PLACEMENT_3D ( 'NONE', #4594, #5496, #7837 ) ;
#3714 = CARTESIAN_POINT ( 'NONE',  ( 1.229367062500000163, -13.00000000000000533, -1.843750000682796708 ) ) ;
#3715 = CARTESIAN_POINT ( 'NONE',  ( 5.697241258616385196, -0.9968613283357656840, -0.5760517167220230439 ) ) ;
#3716 = ADVANCED_FACE ( 'NONE', ( #749 ), #8594, .T. ) ;
#3717 = CARTESIAN_POINT ( 'NONE',  ( 1.229367062500000163, -12.29022459553277002, -0.6770833340161300784 ) ) ;
#3718 = AXIS2_PLACEMENT_3D ( 'NONE', #2851, #5387, #3013 ) ;
#3719 = ORIENTED_EDGE ( 'NONE', *, *, #7077, .T. ) ;
#3720 = STYLED_ITEM ( 'NONE', ( #7505 ), #4735 ) ;
#3721 = LINE ( 'NONE', #545, #858 ) ;
#3722 = CARTESIAN_POINT ( 'NONE',  ( 0.000000000000000000, -7.063614741696270016, 2.343061888689530026 ) ) ;
#3723 = CARTESIAN_POINT ( 'NONE',  ( 1.263368396766194390, -10.00000000000000000, -12.00000000000000000 ) ) ;
#3724 = CARTESIAN_POINT ( 'NONE',  ( -5.999999999999999112, 26.99999999999999289, -14.00000000000000178 ) ) ;
#3725 = ORIENTED_EDGE ( 'NONE', *, *, #5954, .T. ) ;
#3726 = AXIS2_PLACEMENT_3D ( 'NONE', #10017, #7614, #358 ) ;
#3727 = DIRECTION ( 'NONE',  ( 0.000000000000000000, 0.000000000000000000, 1.000000000000000000 ) ) ;
#3728 = AXIS2_PLACEMENT_3D ( 'NONE', #6041, #1287, #2087 ) ;
#3729 = CARTESIAN_POINT ( 'NONE',  ( 3.181980515339458471, 3.181980515339470461, 2.232096619617652273E-17 ) ) ;
#3730 = CARTESIAN_POINT ( 'NONE',  ( -0.6146835312500006365, -14.06466310670085562, -1.510416667349463227 ) ) ;
#3731 = ORIENTED_EDGE ( 'NONE', *, *, #1059, .T. ) ;
#3732 = VECTOR ( 'NONE', #2446, 999.9999999999998863 ) ;
#3733 = ORIENTED_EDGE ( 'NONE', *, *, #287, .T. ) ;
#3734 = EDGE_CURVE ( 'NONE', #2636, #10382, #3815, .T. ) ;
#3735 = CARTESIAN_POINT ( 'NONE',  ( 0.000000000000000000, -13.00000000000000533, -3.000000000000000000 ) ) ;
#3736 = VECTOR ( 'NONE', #3773, 1000.000000000000000 ) ;
#3737 = LINE ( 'NONE', #6966, #4741 ) ;
#3738 = ORIENTED_EDGE ( 'NONE', *, *, #5254, .F. ) ;
#3739 = CARTESIAN_POINT ( 'NONE',  ( 4.940838830814703542, -2.417848759854246410, 7.156051716722023670 ) ) ;
#3740 = CIRCLE ( 'NONE', #9692, 1.600000000000000311 ) ;
#3741 = CARTESIAN_POINT ( 'NONE',  ( 10.00000000000000000, -7.063614741696270016, 2.343061888689530026 ) ) ;
#3742 = ORIENTED_EDGE ( 'NONE', *, *, #3826, .T. ) ;
#3743 = CARTESIAN_POINT ( 'NONE',  ( -1.500000000000000222, -13.00000000000000533, -1.250000000000000000 ) ) ;
#3744 = ORIENTED_EDGE ( 'NONE', *, *, #6863, .F. ) ;
#3745 = PRESENTATION_STYLE_ASSIGNMENT (( #728 ) ) ;
#3746 = ORIENTED_EDGE ( 'NONE', *, *, #3043, .F. ) ;
#3747 = DIRECTION ( 'NONE',  ( -1.000000000000000000, -0.000000000000000000, -0.000000000000000000 ) ) ;
#3748 = PLANE ( 'NONE',  #3045 ) ;
#3749 = ORIENTED_EDGE ( 'NONE', *, *, #4316, .F. ) ;
#3750 = CARTESIAN_POINT ( 'NONE',  ( 0.000000000000000000, 6.000000000000000000, 0.000000000000000000 ) ) ;
#3751 = CARTESIAN_POINT ( 'NONE',  ( 0.000000000000000000, -27.00000000000000711, 0.000000000000000000 ) ) ;
#3752 = CARTESIAN_POINT ( 'NONE',  ( -0.8124729078102072011, 5.726445515403652209, 6.983948283277976010 ) ) ;
#3753 = ORIENTED_EDGE ( 'NONE', *, *, #6802, .T. ) ;
#3754 = DIRECTION ( 'NONE',  ( -1.000000000000000000, 0.000000000000000000, -0.000000000000000000 ) ) ;
#3755 = EDGE_CURVE ( 'NONE', #5890, #4690, #4554, .T. ) ;
#3756 = CARTESIAN_POINT ( 'NONE',  ( 11.00000000000000355, 1.493456771560197319E-16, -1.219500000000000028 ) ) ;
#3757 = CARTESIAN_POINT ( 'NONE',  ( 25.00000000000000000, 0.000000000000000000, -10.00000000000000000 ) ) ;
#3758 = DIRECTION ( 'NONE',  ( -0.000000000000000000, -0.000000000000000000, 1.000000000000000000 ) ) ;
#3759 = PLANE ( 'NONE',  #4067 ) ;
#3760 = FACE_OUTER_BOUND ( 'NONE', #9277, .T. ) ;
#3761 = CARTESIAN_POINT ( 'NONE',  ( 1.263368396766194390, 6.000000000000000000, -12.00000000000000000 ) ) ;
#3762 = ADVANCED_FACE ( 'NONE', ( #2236 ), #3131, .T. ) ;
#3763 = DIRECTION ( 'NONE',  ( 1.000000000000000000, 0.000000000000000000, 0.000000000000000000 ) ) ;
#3764 = CARTESIAN_POINT ( 'NONE',  ( 3.345732310141667387, -3.345732310141653620, 9.099999999999999645 ) ) ;
#3765 = ADVANCED_FACE ( 'NONE', ( #8750 ), #6992, .T. ) ;
#3766 = EDGE_CURVE ( 'NONE', #7393, #8683, #1460, .T. ) ;
#3767 = CARTESIAN_POINT ( 'NONE',  ( 0.6146835312500001924, -11.93533689329915326, -1.760416667349463449 ) ) ;
#3768 = CARTESIAN_POINT ( 'NONE',  ( -2.708615832122950096, -5.110351332421780413, 11.46394828327797555 ) ) ;
#3769 = CARTESIAN_POINT ( 'NONE',  ( -1.229367062500000163, -13.70977540446723708, -1.927083334016129745 ) ) ;
#3770 = EDGE_LOOP ( 'NONE', ( #4414, #760, #10316, #4006, #3428, #609, #3620, #3520, #8615, #976, #2408, #6658 ) ) ;
#3771 = VECTOR ( 'NONE', #1440, 1000.000000000000000 ) ;
#3772 = DIRECTION ( 'NONE',  ( 0.000000000000000000, 0.000000000000000000, 1.000000000000000000 ) ) ;
#3773 = DIRECTION ( 'NONE',  ( 0.000000000000000000, 0.000000000000000000, 1.000000000000000000 ) ) ;
#3774 = FACE_OUTER_BOUND ( 'NONE', #1331, .T. ) ;
#3775 = CARTESIAN_POINT ( 'NONE',  ( 3.000000000000002665, 0.000000000000000000, 2.750000000000000000 ) ) ;
#3776 = ORIENTED_EDGE ( 'NONE', *, *, #10254, .F. ) ;
#3777 = EDGE_CURVE ( 'NONE', #7761, #8717, #6535, .T. ) ;
#3778 = CARTESIAN_POINT ( 'NONE',  ( 10.00000000000000000, 0.000000000000000000, 0.000000000000000000 ) ) ;
#3779 = VECTOR ( 'NONE', #809, 1000.000000000000000 ) ;
#3780 = DIRECTION ( 'NONE',  ( 0.000000000000000000, 0.000000000000000000, 1.000000000000000000 ) ) ;
#3781 = CARTESIAN_POINT ( 'NONE',  ( 4.673326407553653361, -0.7401821875142523544, 0.4199999999999999845 ) ) ;
#3782 = CARTESIAN_POINT ( 'NONE',  ( 1.229367062500000163, -13.00000000000000533, -0.8437500006827965970 ) ) ;
#3783 = ORIENTED_EDGE ( 'NONE', *, *, #4350, .T. ) ;
#3784 = ORIENTED_EDGE ( 'NONE', *, *, #8564, .T. ) ;
#3785 = COLOUR_RGB ( '', 0.09019608, 0.27058824, 0.51372549) ;
#3786 = CARTESIAN_POINT ( 'NONE',  ( 0.1499999999999973577, 0.000000000000000000, 2.750000000000000000 ) ) ;
#3787 = CARTESIAN_POINT ( 'NONE',  ( -2.000000000000012879, 15.00000000000000355, 3.999999999999986233 ) ) ;
#3788 = VERTEX_POINT ( 'NONE', #7212 ) ;
#3789 = CARTESIAN_POINT ( 'NONE',  ( 4.940838830814703542, -2.417848759854246410, 12.75605171672202331 ) ) ;
#3790 = ORIENTED_EDGE ( 'NONE', *, *, #1580, .F. ) ;
#3791 = LINE ( 'NONE', #9431, #4085 ) ;
#3792 = PRODUCT_RELATED_PRODUCT_CATEGORY ( 'part', '', ( #3270 ) ) ;
#3793 = ORIENTED_EDGE ( 'NONE', *, *, #3272, .F. ) ;
#3794 = AXIS2_PLACEMENT_3D ( 'NONE', #7256, #6355, #6458 ) ;
#3795 = ORIENTED_EDGE ( 'NONE', *, *, #2160, .T. ) ;
#3796 = DIRECTION ( 'NONE',  ( 1.000000000000000000, 0.000000000000000000, 0.000000000000000000 ) ) ;
#3797 = VERTEX_POINT ( 'NONE', #9657 ) ;
#3798 = CARTESIAN_POINT ( 'NONE',  ( 9.869213319667256457, 3.750000000000000000, 0.000000000000000000 ) ) ;
#3799 = EDGE_CURVE ( 'NONE', #6026, #7306, #10410, .T. ) ;
#3800 = ORIENTED_EDGE ( 'NONE', *, *, #1033, .F. ) ;
#3801 = DIRECTION ( 'NONE',  ( 0.000000000000000000, 0.000000000000000000, 1.000000000000000000 ) ) ;
#3802 = CARTESIAN_POINT ( 'NONE',  ( -1.500000000000000222, -13.00000000000000533, -1.312500001365593416 ) ) ;
#3803 = CARTESIAN_POINT ( 'NONE',  ( -5.195105386651219348, -2.542276634908102295, 0.5439482832779766186 ) ) ;
#3804 = ORIENTED_EDGE ( 'NONE', *, *, #5876, .T. ) ;
#3805 = AXIS2_PLACEMENT_3D ( 'NONE', #1738, #9207, #10116 ) ;
#3806 = CARTESIAN_POINT ( 'NONE',  ( 1.999999999999986233, 15.00000000000000355, -4.000000000000009770 ) ) ;
#3807 = CARTESIAN_POINT ( 'NONE',  ( 11.30300220323380600, -10.00000000000000000, -12.00000000000000000 ) ) ;
#3808 = PRODUCT_DEFINITION_FORMATION_WITH_SPECIFIED_SOURCE ( 'ANY', '', #3270, .NOT_KNOWN. ) ;
#3809 = CARTESIAN_POINT ( 'NONE',  ( 0.000000000000000000, 0.000000000000000000, -12.00000000000000000 ) ) ;
#3810 = FACE_OUTER_BOUND ( 'NONE', #9958, .T. ) ;
#3811 = AXIS2_PLACEMENT_3D ( 'NONE', #9779, #2507, #4784 ) ;
#3812 = EDGE_CURVE ( 'NONE', #9003, #1372, #7185, .T. ) ;
#3813 = FACE_OUTER_BOUND ( 'NONE', #7936, .T. ) ;
#3814 = DIRECTION ( 'NONE',  ( -0.000000000000000000, -0.000000000000000000, 1.000000000000000000 ) ) ;
#3815 = LINE ( 'NONE', #9505, #7555 ) ;
#3816 = AXIS2_PLACEMENT_3D ( 'NONE', #9085, #4994, #5042 ) ;
#3817 = CARTESIAN_POINT ( 'NONE',  ( -2.000000000000000000, -6.700937042937042065, -2.183447440113260196 ) ) ;
#3818 = CARTESIAN_POINT ( 'NONE',  ( 4.673326407553653361, -0.7401821875142523544, 6.019999999999999574 ) ) ;
#3819 = CARTESIAN_POINT ( 'NONE',  ( -0.6146835312499998594, -11.93533689329915326, -0.5520833340161299674 ) ) ;
#3820 = AXIS2_PLACEMENT_3D ( 'NONE', #646, #10367, #3630 ) ;
#3821 = CARTESIAN_POINT ( 'NONE',  ( -3.951860609387083834, -3.826313983664940466, 8.803948283277977183 ) ) ;
#3822 = CARTESIAN_POINT ( 'NONE',  ( 27.00000000000001066, -31.99999999999998579, 5.999999999999999112 ) ) ;
#3823 = AXIS2_PLACEMENT_3D ( 'NONE', #9559, #3183, #9450 ) ;
#3824 = VERTEX_POINT ( 'NONE', #3980 ) ;
#3825 = APPLICATION_PROTOCOL_DEFINITION ( 'draft international standard', 'automotive_design', 1998, #5599 ) ;
#3826 = EDGE_CURVE ( 'NONE', #7785, #9442, #1383, .T. ) ;
#3827 = CARTESIAN_POINT ( 'NONE',  ( 16.15239861966725599, 3.750000000000000000, -12.00000000000000000 ) ) ;
#3828 = EDGE_CURVE ( 'NONE', #9494, #4339, #4607, .T. ) ;
#3829 = CARTESIAN_POINT ( 'NONE',  ( 1.999999999999984013, 35.00000000000000000, -4.000000000000009770 ) ) ;
#3830 = FACE_OUTER_BOUND ( 'NONE', #3900, .T. ) ;
#3831 = CARTESIAN_POINT ( 'NONE',  ( -3.181725716174720991E-16, -14.73205080756888563, -1.625000000000000222 ) ) ;
#3832 = ORIENTED_EDGE ( 'NONE', *, *, #5450, .T. ) ;
#3833 = CARTESIAN_POINT ( 'NONE',  ( 4.414205890716556446, 6.025400000000000311, 0.000000000000000000 ) ) ;
#3834 = FACE_OUTER_BOUND ( 'NONE', #2049, .T. ) ;
#3835 = CARTESIAN_POINT ( 'NONE',  ( 2.148092372876330369, 4.215868657802593233, 8.259999999999999787 ) ) ;
#3836 = CARTESIAN_POINT ( 'NONE',  ( 1.060575238724907038E-16, -11.26794919243112680, -1.875000000000000222 ) ) ;
#3837 = VERTEX_POINT ( 'NONE', #8015 ) ;
#3838 = EDGE_CURVE ( 'NONE', #8274, #3582, #4771, .T. ) ;
#3839 = ORIENTED_EDGE ( 'NONE', *, *, #4881, .F. ) ;
#3840 = DIRECTION ( 'NONE',  ( 0.000000000000000000, 0.000000000000000000, -1.000000000000000000 ) ) ;
#3841 = CARTESIAN_POINT ( 'NONE',  ( 7.206705994753384914, -12.62302646919798299, 0.000000000000000000 ) ) ;
#3842 = EDGE_LOOP ( 'NONE', ( #6117, #4524, #5236, #1588 ) ) ;
#3843 = CARTESIAN_POINT ( 'NONE',  ( -3.826313983664925811, -3.951860609387098489, 13.59605171672202140 ) ) ;
#3844 = LINE ( 'NONE', #8723, #829 ) ;
#3845 = FILL_AREA_STYLE_COLOUR ( '', #6596 ) ;
#3846 = VERTEX_POINT ( 'NONE', #9718 ) ;
#3847 = CARTESIAN_POINT ( 'NONE',  ( 1.500000000000000222, -12.13397459621556784, -1.520833334698926897 ) ) ;
#3848 = CARTESIAN_POINT ( 'NONE',  ( -2.576046737280769605, 4.860232935257343456, 11.63605171672202232 ) ) ;
#3849 = ORIENTED_EDGE ( 'NONE', *, *, #9352, .F. ) ;
#3850 = EDGE_CURVE ( 'NONE', #8011, #346, #611, .T. ) ;
#3851 = SURFACE_STYLE_FILL_AREA ( #6975 ) ;
#3852 = ORIENTED_EDGE ( 'NONE', *, *, #5378, .F. ) ;
#3853 = DIRECTION ( 'NONE',  ( -0.000000000000000000, -0.000000000000000000, -1.000000000000000000 ) ) ;
#3854 = CARTESIAN_POINT ( 'NONE',  ( 13.82973899676619745, 6.000000000000000000, 0.000000000000000000 ) ) ;
#3855 = VERTEX_POINT ( 'NONE', #4875 ) ;
#3856 = FACE_OUTER_BOUND ( 'NONE', #10349, .T. ) ;
#3857 = DIRECTION ( 'NONE',  ( -0.000000000000000000, -1.000000000000000000, -0.000000000000000000 ) ) ;
#3858 = CARTESIAN_POINT ( 'NONE',  ( -2.708615832122950096, -5.110351332421780413, 3.063948283277976081 ) ) ;
#3859 = ORIENTED_EDGE ( 'NONE', *, *, #6829, .F. ) ;
#3860 = CARTESIAN_POINT ( 'NONE',  ( -0.7499999999999997780, -11.70096189432334555, -1.895833334698926897 ) ) ;
#3861 = CARTESIAN_POINT ( 'NONE',  ( 1.500000000000000222, -12.13397459621556784, -0.5208333346989270085 ) ) ;
#3862 =( NAMED_UNIT ( * ) SI_UNIT ( $, .STERADIAN. ) SOLID_ANGLE_UNIT ( ) );
#3863 = CYLINDRICAL_SURFACE ( 'NONE', #932, 2.399999999999999911 ) ;
#3864 = CARTESIAN_POINT ( 'NONE',  ( 10.00000000000000000, 0.000000000000000000, 0.000000000000000000 ) ) ;
#3865 = CARTESIAN_POINT ( 'NONE',  ( -1.500000000000000222, -13.00000000000000533, -2.250000000000000444 ) ) ;
#3866 = DIRECTION ( 'NONE',  ( 1.000000000000000000, -0.000000000000000000, -0.000000000000000000 ) ) ;
#3867 = DIRECTION ( 'NONE',  ( 0.000000000000000000, 0.000000000000000000, -1.000000000000000000 ) ) ;
#3868 = CARTESIAN_POINT ( 'NONE',  ( 2.042957248827968808, -4.009529358847652603, 3.639999999999999680 ) ) ;
#3869 = AXIS2_PLACEMENT_3D ( 'NONE', #5511, #7372, #5664 ) ;
#3870 = CARTESIAN_POINT ( 'NONE',  ( -1.229367062500000385, -13.70977540446723886, -2.552083334016129967 ) ) ;
#3871 = EDGE_CURVE ( 'NONE', #520, #5053, #5819, .T. ) ;
#3872 = CARTESIAN_POINT ( 'NONE',  ( -3.951860609387083834, -3.826313983664940466, 6.003948283277975584 ) ) ;
#3873 = LINE ( 'NONE', #9565, #3274 ) ;
#3874 = VERTEX_POINT ( 'NONE', #4083 ) ;
#3875 = LINE ( 'NONE', #8921, #10252 ) ;
#3876 = CIRCLE ( 'NONE', #6238, 0.5000000000000000000 ) ;
#3877 = FACE_OUTER_BOUND ( 'NONE', #4533, .T. ) ;
#3878 = CARTESIAN_POINT ( 'NONE',  ( -29.99999999999998934, 1.959434878635763751E-16, -1.599999999999998979 ) ) ;
#3879 = AXIS2_PLACEMENT_3D ( 'NONE', #2224, #5444, #7892 ) ;
#3880 = DIRECTION ( 'NONE',  ( 1.000000000000000000, 0.000000000000000000, 0.000000000000000000 ) ) ;
#3881 = LINE ( 'NONE', #10481, #1195 ) ;
#3882 = ORIENTED_EDGE ( 'NONE', *, *, #2076, .F. ) ;
#3883 = CLOSED_SHELL ( 'NONE', ( #3962, #1480, #4190, #4420, #8088, #7341, #9148, #4823, #4397, #9846, #973, #4623, #3248, #9416, #6165, #10025, #7203, #3706, #3452, #10296, #7401, #1302, #1314, #7176, #3765, #2442, #2348, #1103, #4955, #7660, #7432, #7926, #1555, #8259, #6629, #530, #8863, #8841 ) ) ;
#3884 = FILL_AREA_STYLE ('',( #5472 ) ) ;
#3885 = LINE ( 'NONE', #5577, #9497 ) ;
#3886 = VECTOR ( 'NONE', #6358, 1000.000000000000000 ) ;
#3887 = CARTESIAN_POINT ( 'NONE',  ( 3.345732310141667387, -3.345732310141653620, 9.099999999999999645 ) ) ;
#3888 = UNCERTAINTY_MEASURE_WITH_UNIT (LENGTH_MEASURE( 1.000000000000000082E-05 ), #10391, 'distance_accuracy_value', 'NONE');
#3889 = CARTESIAN_POINT ( 'NONE',  ( 1.500000000000000444, -12.13397459621556607, -1.458333333333333481 ) ) ;
#3890 = ORIENTED_EDGE ( 'NONE', *, *, #9814, .F. ) ;
#3891 = ADVANCED_FACE ( 'NONE', ( #852 ), #4030, .F. ) ;
#3892 = ORIENTED_EDGE ( 'NONE', *, *, #6801, .T. ) ;
#3893 = FACE_OUTER_BOUND ( 'NONE', #367, .T. ) ;
#3894 = AXIS2_PLACEMENT_3D ( 'NONE', #2422, #5639, #4849 ) ;
#3895 = CARTESIAN_POINT ( 'NONE',  ( -1.499999999999997780, -12.13397459621556429, -2.354166668032259935 ) ) ;
#3896 = ORIENTED_EDGE ( 'NONE', *, *, #1681, .F. ) ;
#3897 = CARTESIAN_POINT ( 'NONE',  ( 0.7727076532861471003, 5.446173322633805824, 11.91605171672202346 ) ) ;
#3898 = LINE ( 'NONE', #1576, #7431 ) ;
#3899 = DIRECTION ( 'NONE',  ( 1.000000000000000000, 0.000000000000000000, 0.000000000000000000 ) ) ;
#3900 = EDGE_LOOP ( 'NONE', ( #1885, #5823, #577, #8209 ) ) ;
#3901 = EDGE_CURVE ( 'NONE', #9850, #5808, #4824, .T. ) ;
#3902 = EDGE_CURVE ( 'NONE', #4597, #2608, #8857, .T. ) ;
#3903 = CARTESIAN_POINT ( 'NONE',  ( 4.000000000000000888, 4.058600654062950674, -7.468451026206158083 ) ) ;
#3904 = CARTESIAN_POINT ( 'NONE',  ( -2.542276634908081423, -5.195105386651227342, 10.65605171672202012 ) ) ;
#3905 = AXIS2_PLACEMENT_3D ( 'NONE', #38, #7395, #1829 ) ;
#3906 = ORIENTED_EDGE ( 'NONE', *, *, #2662, .T. ) ;
#3907 =( NAMED_UNIT ( * ) PLANE_ANGLE_UNIT ( ) SI_UNIT ( $, .RADIAN. ) );
#3908 = AXIS2_PLACEMENT_3D ( 'NONE', #1271, #6190, #429 ) ;
#3909 = DIRECTION ( 'NONE',  ( 0.000000000000000000, -0.000000000000000000, 1.000000000000000000 ) ) ;
#3910 = CARTESIAN_POINT ( 'NONE',  ( 8.000000000000001776, -5.233522515400054864, -4.720195129223331065 ) ) ;
#3911 = VECTOR ( 'NONE', #4476, 1000.000000000000000 ) ;
#3912 = EDGE_LOOP ( 'NONE', ( #1502, #8338, #322, #622 ) ) ;
#3913 = DIRECTION ( 'NONE',  ( 0.000000000000000000, 0.000000000000000000, 1.000000000000000000 ) ) ;
#3914 = CARTESIAN_POINT ( 'NONE',  ( -2.000000000000000000, -6.106419733534973915, -3.518755179752866447 ) ) ;
#3915 = CARTESIAN_POINT ( 'NONE',  ( 2.708615832122949652, 5.110351332421781301, 4.463948283277976437 ) ) ;
#3916 = ORIENTED_EDGE ( 'NONE', *, *, #5944, .T. ) ;
#3917 = EDGE_CURVE ( 'NONE', #5731, #6226, #10106, .T. ) ;
#3918 = CARTESIAN_POINT ( 'NONE',  ( -1.500000000000000666, -13.86602540378444459, 0.2291666653010731858 ) ) ;
#3919 = LINE ( 'NONE', #5503, #3446 ) ;
#3920 = PRESENTATION_STYLE_ASSIGNMENT (( #688 ) ) ;
#3921 = EDGE_LOOP ( 'NONE', ( #8999, #7146 ) ) ;
#3922 = AXIS2_PLACEMENT_3D ( 'NONE', #8595, #3763, #3867 ) ;
#3923 = LINE ( 'NONE', #692, #8385 ) ;
#3924 = DIRECTION ( 'NONE',  ( -0.9396926207859105373, -0.3420201433256627732, 0.000000000000000000 ) ) ;
#3925 = DIRECTION ( 'NONE',  ( -0.000000000000000000, -1.000000000000000000, -0.000000000000000000 ) ) ;
#3926 = CARTESIAN_POINT ( 'NONE',  ( -2.000000000000024425, 15.00000000000000355, -5.999999999999988454 ) ) ;
#3927 = DIRECTION ( 'NONE',  ( 1.000000000000000000, 0.000000000000000000, 0.000000000000000000 ) ) ;
#3928 = CARTESIAN_POINT ( 'NONE',  ( -4.444597532678119300, -0.7039550926810477227, 7.279999999999999361 ) ) ;
#3929 = LINE ( 'NONE', #6465, #5262 ) ;
#3930 = CARTESIAN_POINT ( 'NONE',  ( -2.708615832122950096, -5.110351332421780413, 8.663948283277974838 ) ) ;
#3931 = PRODUCT_DEFINITION ( 'UNKNOWN', '', #6341, #5228 ) ;
#3932 = CARTESIAN_POINT ( 'NONE',  ( 0.000000000000000000, 6.000000000000000000, 0.000000000000000000 ) ) ;
#3933 = EDGE_LOOP ( 'NONE', ( #9170, #6733, #6814, #3966 ) ) ;
#3934 = DIRECTION ( 'NONE',  ( -1.000000000000000000, -1.156482317317871478E-16, 5.204170427930421283E-15 ) ) ;
#3935 = LINE ( 'NONE', #7328, #10445 ) ;
#3936 =( BOUNDED_CURVE ( )  B_SPLINE_CURVE ( 2, ( #4587, #564, #8526, #9374, #2006, #8675, #3743 ),
 .UNSPECIFIED., .F., .T. ) 
 B_SPLINE_CURVE_WITH_KNOTS ( ( 3, 2, 2, 3 ),
 ( 0.5000000000000000000, 0.5277777777777777901, 0.5555555555555554692, 0.5833333333333332593 ),
 .UNSPECIFIED. ) 
 CURVE ( )  GEOMETRIC_REPRESENTATION_ITEM ( )  RATIONAL_B_SPLINE_CURVE ( ( 1.000000000000000000, 0.8660254037844387076, 1.000000000000000000, 0.8660254037844387076, 1.000000000000000000, 0.8660254037844392627, 0.9999999999999994449 ) ) 
 REPRESENTATION_ITEM ( '' )  );
#3937 = VERTEX_POINT ( 'NONE', #9770 ) ;
#3938 = CARTESIAN_POINT ( 'NONE',  ( 12.99999999999999645, 19.99999999999999645, -9.000000000000000000 ) ) ;
#3939 = DIRECTION ( 'NONE',  ( 1.000000000000000000, -0.000000000000000000, -0.000000000000000000 ) ) ;
#3940 = CARTESIAN_POINT ( 'NONE',  ( 0.000000000000000000, -13.00000000000000533, -3.000000000000000000 ) ) ;
#3941 = FACE_OUTER_BOUND ( 'NONE', #7990, .T. ) ;
#3942 = DIRECTION ( 'NONE',  ( -0.000000000000000000, -0.000000000000000000, -1.000000000000000000 ) ) ;
#3943 = CARTESIAN_POINT ( 'NONE',  ( -3.345732310141667831, 3.345732310141653620, 13.29999999999999538 ) ) ;
#3944 = AXIS2_PLACEMENT_3D ( 'NONE', #9730, #2462, #5677 ) ;
#3945 = CARTESIAN_POINT ( 'NONE',  ( 1.500000000000000000, -13.86602540378444459, -2.541666666666666963 ) ) ;
#3946 = VERTEX_POINT ( 'NONE', #3339 ) ;
#3947 = VERTEX_POINT ( 'NONE', #1601 ) ;
#3948 = DIRECTION ( 'NONE',  ( -1.000000000000000000, -0.000000000000000000, -0.000000000000000000 ) ) ;
#3949 = EDGE_CURVE ( 'NONE', #201, #6339, #6623, .T. ) ;
#3950 = VECTOR ( 'NONE', #9150, 1000.000000000000000 ) ;
#3951 = DIRECTION ( 'NONE',  ( 0.3420201433256627732, -0.9396926207859105373, 0.000000000000000000 ) ) ;
#3952 = ORIENTED_EDGE ( 'NONE', *, *, #5738, .F. ) ;
#3953 = DIRECTION ( 'NONE',  ( 1.000000000000000000, 0.000000000000000000, 0.000000000000000000 ) ) ;
#3954 = LINE ( 'NONE', #2425, #1345 ) ;
#3955 = ORIENTED_EDGE ( 'NONE', *, *, #9419, .T. ) ;
#3956 = CARTESIAN_POINT ( 'NONE',  ( -2.143395387092215042E-15, -18.24892422621555355, 0.000000000000000000 ) ) ;
#3957 = CARTESIAN_POINT ( 'NONE',  ( -4.687928535947287756, 0.6479879772514611780, 2.816051716722022924 ) ) ;
#3958 = EDGE_LOOP ( 'NONE', ( #4819, #1620, #3212 ) ) ;
#3959 = AXIS2_PLACEMENT_3D ( 'NONE', #6192, #3021, #10348 ) ;
#3960 =( NAMED_UNIT ( * ) PLANE_ANGLE_UNIT ( ) SI_UNIT ( $, .RADIAN. ) );
#3961 = ORIENTED_EDGE ( 'NONE', *, *, #4316, .T. ) ;
#3962 = ADVANCED_FACE ( 'NONE', ( #2499 ), #5712, .F. ) ;
#3963 = CARTESIAN_POINT ( 'NONE',  ( 20.72778015323380529, 6.000000000000000000, -12.00000000000000000 ) ) ;
#3964 = ADVANCED_FACE ( 'NONE', ( #6567 ), #4932, .F. ) ;
#3965 = CARTESIAN_POINT ( 'NONE',  ( -26.99999999999998934, 0.000000000000000000, 0.000000000000000000 ) ) ;
#3966 = ORIENTED_EDGE ( 'NONE', *, *, #5179, .T. ) ;
#3967 = CARTESIAN_POINT ( 'NONE',  ( -2.625446233515515981, -5.152728359536500768, 6.859999999999999432 ) ) ;
#3968 = CARTESIAN_POINT ( 'NONE',  ( -5.999999999999999112, 26.99999999999999289, 3.000000000000000000 ) ) ;
#3969 = CARTESIAN_POINT ( 'NONE',  ( 2.708615832122949652, 5.110351332421781301, 1.663948283277976392 ) ) ;
#3971 = VERTEX_POINT ( 'NONE', #6 ) ;
#3970 = CIRCLE ( 'NONE', #9027, 2.750000000000000000 ) ;
#3972 = CARTESIAN_POINT ( 'NONE',  ( 1.060575238724907038E-16, -11.26794919243112680, -1.437500001365593416 ) ) ;
#3973 = CARTESIAN_POINT ( 'NONE',  ( 30.00000000000001066, -34.99999999999999289, 9.000000000000000000 ) ) ;
#3974 = STYLED_ITEM ( 'NONE', ( #3745 ), #2960 ) ;
#3975 = ORIENTED_EDGE ( 'NONE', *, *, #414, .F. ) ;
#3976 = EDGE_CURVE ( 'NONE', #1830, #145, #1650, .T. ) ;
#3977 = FACE_OUTER_BOUND ( 'NONE', #5477, .T. ) ;
#3978 = DIRECTION ( 'NONE',  ( 1.000000000000000000, 0.000000000000000000, 0.000000000000000000 ) ) ;
#3979 = DIRECTION ( 'NONE',  ( 0.000000000000000000, -0.000000000000000000, 1.000000000000000000 ) ) ;
#3980 = CARTESIAN_POINT ( 'NONE',  ( 0.000000000000000000, -7.750000000000000000, 0.000000000000000000 ) ) ;
#3981 = AXIS2_PLACEMENT_3D ( 'NONE', #3494, #1698, #217 ) ;
#3982 =( REPRESENTATION_RELATIONSHIP ('NONE','NONE', #5100, #8347 ) REPRESENTATION_RELATIONSHIP_WITH_TRANSFORMATION ( #3295 )SHAPE_REPRESENTATION_RELATIONSHIP( ) );
#3983 = CARTESIAN_POINT ( 'NONE',  ( 0.000000000000000000, -27.00000000000000711, -1.249999999999993339 ) ) ;
#3984 = CARTESIAN_POINT ( 'NONE',  ( -4.215868657802586128, -2.148092372876348133, 4.339999999999999858 ) ) ;
#3985 = ORIENTED_EDGE ( 'NONE', *, *, #3261, .F. ) ;
#3986 = LINE ( 'NONE', #7217, #10179 ) ;
#3987 = CARTESIAN_POINT ( 'NONE',  ( -2.417848759854264618, 4.940838830814694660, 9.643948283277975264 ) ) ;
#3988 = DIRECTION ( 'NONE',  ( 1.000000000000000000, 0.000000000000000000, 0.000000000000000000 ) ) ;
#3989 = VECTOR ( 'NONE', #4859, 1000.000000000000000 ) ;
#3990 = ORIENTED_EDGE ( 'NONE', *, *, #8095, .F. ) ;
#3991 = CONTEXT_DEPENDENT_SHAPE_REPRESENTATION ( #4709, #8100 ) ;
#3992 = CARTESIAN_POINT ( 'NONE',  ( 5.711843387010019590, -0.9046671180729753958, 0.4199999999999999289 ) ) ;
#3993 = LINE ( 'NONE', #3298, #9934 ) ;
#3994 = ORIENTED_EDGE ( 'NONE', *, *, #5376, .T. ) ;
#3995 = FACE_OUTER_BOUND ( 'NONE', #8090, .T. ) ;
#3996 = CARTESIAN_POINT ( 'NONE',  ( 30.00000000000001066, -25.00000000000000000, 0.000000000000000000 ) ) ;
#3997 = DIRECTION ( 'NONE',  ( 1.000000000000000000, 0.000000000000000000, 0.000000000000000000 ) ) ;
#3998 = AXIS2_PLACEMENT_3D ( 'NONE', #1610, #8132, #759 ) ;
#3999 = PRESENTATION_STYLE_ASSIGNMENT (( #2568 ) ) ;
#4000 = FACE_OUTER_BOUND ( 'NONE', #3933, .T. ) ;
#4001 = AXIS2_PLACEMENT_3D ( 'NONE', #9354, #2036, #2090 ) ;
#4002 = CARTESIAN_POINT ( 'NONE',  ( -3.181980515339458027, -3.181980515339470905, 12.59999999999999787 ) ) ;
#4003 = UNCERTAINTY_MEASURE_WITH_UNIT (LENGTH_MEASURE( 1.000000000000000082E-05 ), #5649, 'distance_accuracy_value', 'NONE');
#4004 = CARTESIAN_POINT ( 'NONE',  ( -1.500000000000000666, -13.86602540378444459, -0.7083333333333333703 ) ) ;
#4005 = ORIENTED_EDGE ( 'NONE', *, *, #9069, .F. ) ;
#4006 = ORIENTED_EDGE ( 'NONE', *, *, #2129, .F. ) ;
#4007 = CARTESIAN_POINT ( 'NONE',  ( -1.500000000000000222, -13.00000000000000533, -0.7500000000000002220 ) ) ;
#4008 = CARTESIAN_POINT ( 'NONE',  ( 3.889087296526005488, 3.889087296526018811, 13.99999999999999822 ) ) ;
#4009 = ADVANCED_FACE ( 'NONE', ( #9818 ), #9073, .F. ) ;
#4010 = ORIENTED_EDGE ( 'NONE', *, *, #2543, .T. ) ;
#4011 = CARTESIAN_POINT ( 'NONE',  ( -2.042957248827969252, 4.009529358847651714, 2.239999999999999769 ) ) ;
#4012 = ORIENTED_EDGE ( 'NONE', *, *, #1723, .T. ) ;
#4013 = CARTESIAN_POINT ( 'NONE',  ( 5.726445515403654873, -0.8124729078101852187, 12.61605171672202097 ) ) ;
#4014 = EDGE_CURVE ( 'NONE', #8882, #10462, #8279, .T. ) ;
#4015 = ORIENTED_EDGE ( 'NONE', *, *, #9970, .F. ) ;
#4016 = ORIENTED_EDGE ( 'NONE', *, *, #7981, .T. ) ;
#4017 = DIRECTION ( 'NONE',  ( 0.000000000000000000, 0.000000000000000000, 1.000000000000000000 ) ) ;
#4018 = CARTESIAN_POINT ( 'NONE',  ( -1.500000000000000222, -13.00000000000000533, -1.750000000000000000 ) ) ;
#4019 = ORIENTED_EDGE ( 'NONE', *, *, #4025, .T. ) ;
#4020 = CARTESIAN_POINT ( 'NONE',  ( 2.496947748567516889, -4.900535883036019946, 6.439999999999999503 ) ) ;
#4021 = DIRECTION ( 'NONE',  ( 0.3420201433256627732, -0.9396926207859105373, 0.000000000000000000 ) ) ;
#4022 = CARTESIAN_POINT ( 'NONE',  ( 2.625446233515515537, 5.152728359536502545, 2.659999999999998366 ) ) ;
#4023 = ORIENTED_EDGE ( 'NONE', *, *, #1815, .T. ) ;
#4024 = CARTESIAN_POINT ( 'NONE',  ( -3.181725716174720498E-16, -14.73205080756888385, -0.6875000013655935271 ) ) ;
#4025 = EDGE_CURVE ( 'NONE', #3169, #2333, #1523, .T. ) ;
#4026 = ORIENTED_EDGE ( 'NONE', *, *, #4757, .F. ) ;
#4027 = LINE ( 'NONE', #3076, #1270 ) ;
#4028 = PLANE ( 'NONE',  #8996 ) ;
#4029 = CARTESIAN_POINT ( 'NONE',  ( 0.7499999999999991118, -14.29903810567666333, -2.083333333333333481 ) ) ;
#4030 = PLANE ( 'NONE',  #2818 ) ;
#4031 = FACE_OUTER_BOUND ( 'NONE', #9142, .T. ) ;
#4032 = CARTESIAN_POINT ( 'NONE',  ( -0.6479879772514802738, 4.687928535947285091, 4.183948283277976188 ) ) ;
#4033 = EDGE_LOOP ( 'NONE', ( #8278, #7652, #2092, #9801 ) ) ;
#4034 = CARTESIAN_POINT ( 'NONE',  ( 5.838749930332745919, -7.750000000000000000, -12.00000000000000000 ) ) ;
#4035 = ADVANCED_FACE ( 'NONE', ( #8226 ), #4185, .F. ) ;
#4036 = EDGE_CURVE ( 'NONE', #8297, #2636, #162, .T. ) ;
#4037 = CARTESIAN_POINT ( 'NONE',  ( 5.711843387010018702, -0.9046671180729751738, 6.019999999999999574 ) ) ;
#4038 = CARTESIAN_POINT ( 'NONE',  ( 27.00000000000001066, -31.99999999999998579, 9.000000000000000000 ) ) ;
#4039 = PRODUCT_CONTEXT ( 'NONE', #8858, 'mechanical' ) ;
#4040 = CARTESIAN_POINT ( 'NONE',  ( 2.625446233515515093, 5.152728359536503433, 2.659999999999999254 ) ) ;
#4041 = FACE_OUTER_BOUND ( 'NONE', #1791, .T. ) ;
#4042 = CARTESIAN_POINT ( 'NONE',  ( 18.40512053033274853, -7.750000000000000000, 0.000000000000000000 ) ) ;
#4043 = CARTESIAN_POINT ( 'NONE',  ( 23.26376179071655770, 6.025400000000000311, -12.00000000000000000 ) ) ;
#4044 = PLANE ( 'NONE',  #2540 ) ;
#4045 = LINE ( 'NONE', #9838, #10321 ) ;
#4046 = LINE ( 'NONE', #714, #2384 ) ;
#4047 = EDGE_CURVE ( 'NONE', #9691, #4320, #8071, .T. ) ;
#4048 = CARTESIAN_POINT ( 'NONE',  ( 0.7916369971161419938, 4.430710083317576320, 4.323948283277975868 ) ) ;
#4049 = CARTESIAN_POINT ( 'NONE',  ( -1.500000000000000000, -12.13397459621556607, -0.7916666666666666297 ) ) ;
#4050 = ORIENTED_EDGE ( 'NONE', *, *, #3577, .F. ) ;
#4051 = ORIENTED_EDGE ( 'NONE', *, *, #7, .F. ) ;
#4052 = LINE ( 'NONE', #822, #4927 ) ;
#4053 = CARTESIAN_POINT ( 'NONE',  ( 10.00000000000000000, -6.200809695932781196, 0.7745709230444935978 ) ) ;
#4054 = EDGE_LOOP ( 'NONE', ( #1910, #8994, #3258, #1361 ) ) ;
#4055 = AXIS2_PLACEMENT_3D ( 'NONE', #6666, #219, #3495 ) ;
#4056 = CARTESIAN_POINT ( 'NONE',  ( 3.345732310141667387, -3.345732310141654064, 3.499999999999999112 ) ) ;
#4057 = DIRECTION ( 'NONE',  ( 0.000000000000000000, -0.000000000000000000, 1.000000000000000000 ) ) ;
#4058 = ORIENTED_EDGE ( 'NONE', *, *, #1767, .F. ) ;
#4059 = VECTOR ( 'NONE', #8888, 1000.000000000000000 ) ;
#4060 = EDGE_CURVE ( 'NONE', #5694, #9178, #8533, .T. ) ;
#4061 = CARTESIAN_POINT ( 'NONE',  ( -3.826313983664925811, -3.951860609387098489, 13.59605171672202140 ) ) ;
#4062 = ORIENTED_EDGE ( 'NONE', *, *, #8126, .T. ) ;
#4063 =( NAMED_UNIT ( * ) SI_UNIT ( $, .STERADIAN. ) SOLID_ANGLE_UNIT ( ) );
#4064 =( GEOMETRIC_REPRESENTATION_CONTEXT ( 3 ) GLOBAL_UNCERTAINTY_ASSIGNED_CONTEXT ( ( #1569 ) ) GLOBAL_UNIT_ASSIGNED_CONTEXT ( ( #5698, #8265, #255 ) ) REPRESENTATION_CONTEXT ( 'NONE', 'WORKASPACE' ) );
#4065 = ORIENTED_EDGE ( 'NONE', *, *, #6093, .T. ) ;
#4066 = CARTESIAN_POINT ( 'NONE',  ( 30.00000000000001066, 0.000000000000000000, -1.599999999999992983 ) ) ;
#4067 = AXIS2_PLACEMENT_3D ( 'NONE', #634, #3023, #694 ) ;
#4068 = CARTESIAN_POINT ( 'NONE',  ( -29.99999999999998934, -13.00000000000000533, -1.249999999999987121 ) ) ;
#4069 = ORIENTED_EDGE ( 'NONE', *, *, #6660, .F. ) ;
#4070 = CARTESIAN_POINT ( 'NONE',  ( -0.9046671180729963790, 5.711843387010016926, 7.979999999999999538 ) ) ;
#4071 = CARTESIAN_POINT ( 'NONE',  ( 10.00000000000000000, -0.1221666339523208161, -6.247805719894685694 ) ) ;
#4072 = CARTESIAN_POINT ( 'NONE',  ( 0.9480714621563713917, 5.418398423912717199, 9.923948283277976401 ) ) ;
#4073 = EDGE_LOOP ( 'NONE', ( #10105, #8361, #5226, #8583 ) ) ;
#4074 = AXIS2_PLACEMENT_3D ( 'NONE', #4953, #8199, #9848 ) ;
#4075 = CARTESIAN_POINT ( 'NONE',  ( -1.500000000000000222, -13.00000000000000533, 0.1874999986344063341 ) ) ;
#4076 = VECTOR ( 'NONE', #7054, 1000.000000000000000 ) ;
#4077 = CIRCLE ( 'NONE', #357, 1.280000000000000027 ) ;
#4078 = VERTEX_POINT ( 'NONE', #9175 ) ;
#4079 = CIRCLE ( 'NONE', #10360, 1.249999999999997558 ) ;
#4080 = AXIS2_PLACEMENT_3D ( 'NONE', #5316, #7760, #7599 ) ;
#4081 = CARTESIAN_POINT ( 'NONE',  ( 5.999999999999999112, 26.99999999999999289, -14.00000000000000178 ) ) ;
#4082 = DIRECTION ( 'NONE',  ( 1.000000000000000000, 0.000000000000000000, 0.000000000000000000 ) ) ;
#4083 = CARTESIAN_POINT ( 'NONE',  ( 5.838749930332745919, -7.750000000000000000, 0.000000000000000000 ) ) ;
#4084 = EDGE_CURVE ( 'NONE', #3946, #7840, #4896, .T. ) ;
#4085 = VECTOR ( 'NONE', #10173, 1000.000000000000000 ) ;
#4086 = CARTESIAN_POINT ( 'NONE',  ( -2.000000000000000000, 0.000000000000000000, 0.000000000000000000 ) ) ;
#4087 = CARTESIAN_POINT ( 'NONE',  ( -3.345732310141667831, 3.345732310141653620, 13.29999999999999538 ) ) ;
#4088 = ORIENTED_EDGE ( 'NONE', *, *, #2734, .T. ) ;
#4089 = CARTESIAN_POINT ( 'NONE',  ( -1.229367062500000385, -13.70977540446723886, -0.5520833340161299674 ) ) ;
#4090 = AXIS2_PLACEMENT_3D ( 'NONE', #5888, #8987, #2625 ) ;
#4091 = CARTESIAN_POINT ( 'NONE',  ( -2.496947748567517333, 4.900535883036019058, 5.039999999999999147 ) ) ;
#4092 = DIRECTION ( 'NONE',  ( 0.000000000000000000, -7.993605777301128669E-15, -1.000000000000000000 ) ) ;
#4093 = LINE ( 'NONE', #7327, #1360 ) ;
#4094 = CARTESIAN_POINT ( 'NONE',  ( 4.414205890716556446, 6.025400000000000311, -12.00000000000000000 ) ) ;
#4095 = EDGE_CURVE ( 'NONE', #138, #6440, #6823, .T. ) ;
#4096 = LINE ( 'NONE', #125, #2647 ) ;
#4097 = EDGE_CURVE ( 'NONE', #9757, #1996, #3597, .T. ) ;
#4098 = DIRECTION ( 'NONE',  ( -1.000000000000000000, 0.000000000000000000, 0.000000000000000000 ) ) ;
#4099 = LINE ( 'NONE', #6374, #5736 ) ;
#4100 = CARTESIAN_POINT ( 'NONE',  ( -4.173491630687863108, -2.231261971483782691, 8.136051716722024096 ) ) ;
#4101 = CARTESIAN_POINT ( 'NONE',  ( 1.300000000000000044, 0.7390083445627193548, -1.280000000000000693 ) ) ;
#4102 = FACE_OUTER_BOUND ( 'NONE', #7464, .T. ) ;
#4103 = CARTESIAN_POINT ( 'NONE',  ( 0.7916369971161419938, 4.430710083317576320, 7.123948283277974802 ) ) ;
#4104 = CARTESIAN_POINT ( 'NONE',  ( 0.000000000000000000, 26.99999999999999289, 0.000000000000000000 ) ) ;
#4105 = VERTEX_POINT ( 'NONE', #5919 ) ;
#4106 = ORIENTED_EDGE ( 'NONE', *, *, #4133, .F. ) ;
#4107 = ADVANCED_FACE ( 'NONE', ( #7686 ), #10080, .T. ) ;
#4108 = DIRECTION ( 'NONE',  ( 1.000000000000000000, 0.000000000000000000, 0.000000000000000000 ) ) ;
#4109 = DIRECTION ( 'NONE',  ( 1.000000000000000000, 0.000000000000000000, 0.000000000000000000 ) ) ;
#4110 = ORIENTED_EDGE ( 'NONE', *, *, #2254, .F. ) ;
#4111 = CARTESIAN_POINT ( 'NONE',  ( 3.345732310141667387, -3.345732310141654064, 0.6999999999999997335 ) ) ;
#4112 = ORIENTED_EDGE ( 'NONE', *, *, #9268, .T. ) ;
#4113 = CARTESIAN_POINT ( 'NONE',  ( -4.687928535947287756, 0.6479879772514611780, 5.616051716722022746 ) ) ;
#4114 = ORIENTED_EDGE ( 'NONE', *, *, #1991, .F. ) ;
#4115 = VERTEX_POINT ( 'NONE', #2699 ) ;
#4116 = AXIS2_PLACEMENT_3D ( 'NONE', #7220, #9456, #8654 ) ;
#4117 = DIRECTION ( 'NONE',  ( 0.7071067811865467956, 0.7071067811865484609, -6.099057733344262077E-17 ) ) ;
#4118 = SURFACE_STYLE_USAGE ( .BOTH. , #1739 ) ;
#4119 = ORIENTED_EDGE ( 'NONE', *, *, #2513, .T. ) ;
#4120 = CARTESIAN_POINT ( 'NONE',  ( -3.889087296526005044, -3.889087296526019255, 1.399999999999999689 ) ) ;
#4121 = CARTESIAN_POINT ( 'NONE',  ( -2.496947748567517333, 4.900535883036019058, 5.039999999999999147 ) ) ;
#4122 = CARTESIAN_POINT ( 'NONE',  ( -2.625446233515515981, -5.152728359536500768, 1.259999999999999787 ) ) ;
#4123 = ORIENTED_EDGE ( 'NONE', *, *, #10148, .T. ) ;
#4124 = CARTESIAN_POINT ( 'NONE',  ( 1.500000000000000000, -13.86602540378444459, -1.104166668032260379 ) ) ;
#4125 =( NAMED_UNIT ( * ) SI_UNIT ( $, .STERADIAN. ) SOLID_ANGLE_UNIT ( ) );
#4126 = ORIENTED_EDGE ( 'NONE', *, *, #6482, .T. ) ;
#4127 = LINE ( 'NONE', #7367, #9402 ) ;
#4128 = CARTESIAN_POINT ( 'NONE',  ( 1.364683531250000303, -13.00000000000000533, 0.07812499965860171536 ) ) ;
#4129 = DIRECTION ( 'NONE',  ( 0.000000000000000000, 0.000000000000000000, 1.000000000000000000 ) ) ;
#4130 = CIRCLE ( 'NONE', #5480, 8.500000000000000000 ) ;
#4131 = DIRECTION ( 'NONE',  ( 1.000000000000000000, 0.000000000000000000, -0.000000000000000000 ) ) ;
#4132 = CARTESIAN_POINT ( 'NONE',  ( 25.57717656966725883, 3.750000000000000000, -12.00000000000000000 ) ) ;
#4133 = EDGE_CURVE ( 'NONE', #4614, #5123, #168, .T. ) ;
#4134 = CARTESIAN_POINT ( 'NONE',  ( -3.181980515339458027, -3.181980515339470905, 12.59999999999999787 ) ) ;
#4135 = ORIENTED_EDGE ( 'NONE', *, *, #10174, .T. ) ;
#4136 = CARTESIAN_POINT ( 'NONE',  ( 8.692241771943169307E-17, -11.58044919106553294, -0.7187500006827969301 ) ) ;
#4137 = CARTESIAN_POINT ( 'NONE',  ( 0.8603895577212593571, 5.432285873273261068, 5.319999999999999396 ) ) ;
#4138 =( GEOMETRIC_REPRESENTATION_CONTEXT ( 3 ) GLOBAL_UNCERTAINTY_ASSIGNED_CONTEXT ( ( #10375 ) ) GLOBAL_UNIT_ASSIGNED_CONTEXT ( ( #9434, #3907, #6336 ) ) REPRESENTATION_CONTEXT ( 'NONE', 'WORKASPACE' ) );
#4139 = DIRECTION ( 'NONE',  ( 1.000000000000000000, 0.000000000000000000, 0.000000000000000000 ) ) ;
#4140 = EDGE_CURVE ( 'NONE', #980, #2738, #5397, .T. ) ;
#4141 = CARTESIAN_POINT ( 'NONE',  ( 2.496947748567516889, -4.900535883036019946, 3.639999999999999680 ) ) ;
#4142 = AXIS2_PLACEMENT_3D ( 'NONE', #2125, #7797, #1322 ) ;
#4143 = CARTESIAN_POINT ( 'NONE',  ( 0.000000000000000000, 6.000000000000000000, 0.000000000000000000 ) ) ;
#4144 = FACE_OUTER_BOUND ( 'NONE', #7522, .T. ) ;
#4145 = AXIS2_PLACEMENT_3D ( 'NONE', #1893, #1995, #2786 ) ;
#4146 = DIRECTION ( 'NONE',  ( 0.3420201433256627732, 0.9396926207859105373, 0.000000000000000000 ) ) ;
#4147 = DIRECTION ( 'NONE',  ( 0.000000000000000000, 0.000000000000000000, 1.000000000000000000 ) ) ;
#4148 = CARTESIAN_POINT ( 'NONE',  ( -3.411736077305382420, 3.279728542977939476, 3.096051716722023617 ) ) ;
#4149 = DIRECTION ( 'NONE',  ( 0.7043149233066460235, -0.7043149233066438031, 0.08877487040322794287 ) ) ;
#4150 = CIRCLE ( 'NONE', #2974, 3.000000000000000000 ) ;
#4151 = CARTESIAN_POINT ( 'NONE',  ( -3.969226411068985882, 2.122056237541205537, 3.763948283277976703 ) ) ;
#4152 = EDGE_CURVE ( 'NONE', #7510, #4614, #8620, .T. ) ;
#4153 = LINE ( 'NONE', #975, #4285 ) ;
#4154 = ADVANCED_FACE ( 'NONE', ( #4335 ), #1062, .F. ) ;
#4155 = EDGE_LOOP ( 'NONE', ( #5918, #8662, #7720, #10432 ) ) ;
#4156 = VERTEX_POINT ( 'NONE', #7574 ) ;
#4157 = DIRECTION ( 'NONE',  ( 0.000000000000000000, 0.000000000000000000, 1.000000000000000000 ) ) ;
#4158 = AXIS2_PLACEMENT_3D ( 'NONE', #124, #2298, #5522 ) ;
#4159 = CARTESIAN_POINT ( 'NONE',  ( 13.01080596966725622, 3.750000000000000000, -12.00000000000000000 ) ) ;
#4160 = EDGE_LOOP ( 'NONE', ( #9061, #9473, #6603 ) ) ;
#4161 = VECTOR ( 'NONE', #6144, 1000.000000000000000 ) ;
#4162 = SURFACE_SIDE_STYLE ('',( #5742 ) ) ;
#4163 = ORIENTED_EDGE ( 'NONE', *, *, #4922, .T. ) ;
#4164 = CARTESIAN_POINT ( 'NONE',  ( 0.6162731882459174804, 4.458484982038668498, 6.316051716722022924 ) ) ;
#4165 = EDGE_CURVE ( 'NONE', #2377, #7824, #5081, .T. ) ;
#4166 = CARTESIAN_POINT ( 'NONE',  ( 0.7499999999999991118, -14.29903810567666333, -1.145833334698926897 ) ) ;
#4167 = ORIENTED_EDGE ( 'NONE', *, *, #4732, .F. ) ;
#4168 = VECTOR ( 'NONE', #7319, 1000.000000000000000 ) ;
#4169 = VERTEX_POINT ( 'NONE', #6669 ) ;
#4170 = CARTESIAN_POINT ( 'NONE',  ( 1.500000000000000222, -13.00000000000000533, -2.781250000682796486 ) ) ;
#4171 = LINE ( 'NONE', #2638, #2204 ) ;
#4172 = VERTEX_POINT ( 'NONE', #9925 ) ;
#4173 = CARTESIAN_POINT ( 'NONE',  ( 5.432285873273257515, 0.8603895577212793411, 5.879999999999999893 ) ) ;
#4174 = CARTESIAN_POINT ( 'NONE',  ( -5.432285873273256627, -0.8603895577212797852, 7.279999999999999361 ) ) ;
#4175 = CARTESIAN_POINT ( 'NONE',  ( -3.889087296526005044, -3.889087296526019255, 4.200000000000000178 ) ) ;
#4176 = ORIENTED_EDGE ( 'NONE', *, *, #7488, .F. ) ;
#4177 = CARTESIAN_POINT ( 'NONE',  ( 1.229367062500000385, -12.29022459553277002, -1.677083334016129967 ) ) ;
#4178 = EDGE_CURVE ( 'NONE', #6828, #9702, #5968, .T. ) ;
#4179 = APPLICATION_CONTEXT ( 'automotive_design' ) ;
#4180 = ORIENTED_EDGE ( 'NONE', *, *, #5783, .T. ) ;
#4181 = DIRECTION ( 'NONE',  ( 0.9396926207859105373, 0.3420201433256627732, 0.000000000000000000 ) ) ;
#4182 = CARTESIAN_POINT ( 'NONE',  ( 23.86012795928344588, 6.025400000000000311, -12.00000000000000000 ) ) ;
#4183 = DIRECTION ( 'NONE',  ( 1.000000000000000000, 0.000000000000000000, 0.000000000000000000 ) ) ;
#4184 = ORIENTED_EDGE ( 'NONE', *, *, #8126, .F. ) ;
#4185 = PLANE ( 'NONE',  #333 ) ;
#4186 = CARTESIAN_POINT ( 'NONE',  ( 1.229367062500000163, -13.70977540446723886, -0.8854166673494634487 ) ) ;
#4187 = CARTESIAN_POINT ( 'NONE',  ( 4.458484982038663169, 0.6162731882459350219, 4.883948283277976365 ) ) ;
#4188 = ORIENTED_EDGE ( 'NONE', *, *, #2871, .F. ) ;
#4189 = FACE_OUTER_BOUND ( 'NONE', #7953, .T. ) ;
#4190 = ADVANCED_FACE ( 'NONE', ( #2806 ), #6878, .F. ) ;
#4191 = CARTESIAN_POINT ( 'NONE',  ( 5.152728359536493663, 2.625446233515533745, 2.939999999999999059 ) ) ;
#4192 = DIRECTION ( 'NONE',  ( 0.000000000000000000, 0.000000000000000000, 1.000000000000000000 ) ) ;
#4193 = CARTESIAN_POINT ( 'NONE',  ( -2.496947748567517333, 4.900535883036019058, 5.039999999999999147 ) ) ;
#4194 = DIRECTION ( 'NONE',  ( -1.000000000000000000, -4.625929269271485914E-16, 0.000000000000000000 ) ) ;
#4195 = CARTESIAN_POINT ( 'NONE',  ( 14.44459485323380576, -10.00000000000000000, -12.00000000000000000 ) ) ;
#4196 = CARTESIAN_POINT ( 'NONE',  ( 1.364683531250000303, -13.00000000000000533, -2.921875000341398465 ) ) ;
#4197 = CARTESIAN_POINT ( 'NONE',  ( 2.122056237541221524, -3.969226411068978777, 7.436051716722023031 ) ) ;
#4198 = EDGE_CURVE ( 'NONE', #1471, #6291, #7526, .T. ) ;
#4199 = FACE_OUTER_BOUND ( 'NONE', #7216, .T. ) ;
#4200 = CARTESIAN_POINT ( 'NONE',  ( 0.6479879772514793856, -4.687928535947285091, 8.383948283277975477 ) ) ;
#4201 = LINE ( 'NONE', #9136, #8193 ) ;
#4202 = ORIENTED_EDGE ( 'NONE', *, *, #5192, .T. ) ;
#4203 = CARTESIAN_POINT ( 'NONE',  ( -5.110351332421769754, -2.708615832122969191, 2.536051716722023119 ) ) ;
#4204 = LINE ( 'NONE', #9094, #1890 ) ;
#4205 = DIRECTION ( 'NONE',  ( 0.000000000000000000, 0.000000000000000000, -1.000000000000000000 ) ) ;
#4206 = ORIENTED_EDGE ( 'NONE', *, *, #8101, .F. ) ;
#4207 = EDGE_CURVE ( 'NONE', #9761, #3093, #2368, .T. ) ;
#4208 = CARTESIAN_POINT ( 'NONE',  ( 1.500000000000000222, -13.00000000000000533, 0.2187499993172032642 ) ) ;
#4209 = ORIENTED_EDGE ( 'NONE', *, *, #1158, .T. ) ;
#4210 = CIRCLE ( 'NONE', #3532, 3.000000000000000444 ) ;
#4211 = CARTESIAN_POINT ( 'NONE',  ( 4.049832306626335310, -1.963858260114701215, 4.356051716722023848 ) ) ;
#4212 = CARTESIAN_POINT ( 'NONE',  ( 3.586028019667255595, 3.750000000000000000, -12.00000000000000000 ) ) ;
#4213 = ORIENTED_EDGE ( 'NONE', *, *, #4717, .T. ) ;
#4214 = FILL_AREA_STYLE ('',( #2529 ) ) ;
#4215 = VERTEX_POINT ( 'NONE', #1266 ) ;
#4216 = DIRECTION ( 'NONE',  ( -0.000000000000000000, -0.000000000000000000, -1.000000000000000000 ) ) ;
#4217 = AXIS2_PLACEMENT_3D ( 'NONE', #6959, #1293, #4519 ) ;
#4218 = DIRECTION ( 'NONE',  ( -1.156482317317871478E-16, 1.000000000000000000, 0.000000000000000000 ) ) ;
#4219 = ORIENTED_EDGE ( 'NONE', *, *, #8738, .T. ) ;
#4220 = ADVANCED_FACE ( 'NONE', ( #8482 ), #1215, .F. ) ;
#4221 = AXIS2_PLACEMENT_3D ( 'NONE', #3445, #5133, #10033 ) ;
#4222 = CARTESIAN_POINT ( 'NONE',  ( -2.496947748567517333, 4.900535883036019058, 13.43999999999999950 ) ) ;
#4223 = ADVANCED_FACE ( 'NONE', ( #5291 ), #4492, .T. ) ;
#4224 = CARTESIAN_POINT ( 'NONE',  ( -5.152728359536494551, -2.625446233515535077, 4.339999999999999858 ) ) ;
#4225 = CARTESIAN_POINT ( 'NONE',  ( 4.089228379062037178, -4.089228379062022967, 3.499999999999998668 ) ) ;
#4226 = ORIENTED_EDGE ( 'NONE', *, *, #2678, .T. ) ;
#4227 = CARTESIAN_POINT ( 'NONE',  ( -1.229367062500000163, -13.00000000000000533, -1.968750000682796708 ) ) ;
#4228 = AXIS2_PLACEMENT_3D ( 'NONE', #3910, #5442, #7136 ) ;
#4229 = ORIENTED_EDGE ( 'NONE', *, *, #4640, .T. ) ;
#4230 = CARTESIAN_POINT ( 'NONE',  ( 5.999999999999999112, -27.00000000000000711, 3.000000000000000000 ) ) ;
#4231 = CARTESIAN_POINT ( 'NONE',  ( -1.500000000000000222, -13.00000000000000533, -3.000000000000000000 ) ) ;
#4232 = ORIENTED_EDGE ( 'NONE', *, *, #9554, .T. ) ;
#4233 = EDGE_CURVE ( 'NONE', #2939, #409, #10398, .T. ) ;
#4234 = DIRECTION ( 'NONE',  ( 0.000000000000000000, 1.000000000000000000, 0.000000000000000000 ) ) ;
#4235 = STYLED_ITEM ( 'NONE', ( #8670 ), #8241 ) ;
#4236 = CARTESIAN_POINT ( 'NONE',  ( -0.6146835312499998594, -11.93533689329915326, -0.6770833340161300784 ) ) ;
#4237 = CARTESIAN_POINT ( 'NONE',  ( -0.7039550926810301812, -4.444597532678121965, 12.31999999999999851 ) ) ;
#4238 = VERTEX_POINT ( 'NONE', #10234 ) ;
#4239 = LINE ( 'NONE', #8283, #2886 ) ;
#4240 = CIRCLE ( 'NONE', #3908, 6.248999999999999666 ) ;
#4241 = CARTESIAN_POINT ( 'NONE',  ( 5.432285873273257515, 0.8603895577212793411, 5.879999999999999893 ) ) ;
#4242 = DIRECTION ( 'NONE',  ( 0.000000000000000000, 1.000000000000000000, 0.000000000000000000 ) ) ;
#4243 = CARTESIAN_POINT ( 'NONE',  ( -0.8603895577212598011, -5.432285873273260179, 9.519999999999999574 ) ) ;
#4244 = DIRECTION ( 'NONE',  ( 0.000000000000000000, 0.000000000000000000, 1.000000000000000000 ) ) ;
#4245 = CARTESIAN_POINT ( 'NONE',  ( 0.000000000000000000, -13.00000000000000533, -3.000000000000000000 ) ) ;
#4246 = VECTOR ( 'NONE', #2936, 1000.000000000000000 ) ;
#4247 = CARTESIAN_POINT ( 'NONE',  ( -26.99999999999998934, 34.99999999999999289, -5.999999999999999112 ) ) ;
#4248 = CARTESIAN_POINT ( 'NONE',  ( 0.6162731882459174804, 4.458484982038668498, 3.516051716722023102 ) ) ;
#4249 = CARTESIAN_POINT ( 'NONE',  ( 1.229367062500000163, -13.00000000000000533, -1.718750000682796486 ) ) ;
#4250 = CARTESIAN_POINT ( 'NONE',  ( -4.658724279160018078, 0.8323763977770419764, 6.423948283277978177 ) ) ;
#4251 = CARTESIAN_POINT ( 'NONE',  ( -1.229367062500000163, -12.29022459553277002, -2.510416667349463449 ) ) ;
#4252 = VERTEX_POINT ( 'NONE', #4697 ) ;
#4253 = CARTESIAN_POINT ( 'NONE',  ( 0.7727076532861471003, 5.446173322633805824, 6.316051716722022924 ) ) ;
#4254 = EDGE_CURVE ( 'NONE', #4487, #6626, #521, .T. ) ;
#4255 = FACE_OUTER_BOUND ( 'NONE', #1674, .T. ) ;
#4256 = FACE_OUTER_BOUND ( 'NONE', #1056, .T. ) ;
#4257 = ORIENTED_EDGE ( 'NONE', *, *, #3136, .F. ) ;
#4258 = CARTESIAN_POINT ( 'NONE',  ( -2.042957248827969252, 4.009529358847651714, 10.63999999999999879 ) ) ;
#4259 = SURFACE_STYLE_USAGE ( .BOTH. , #1938 ) ;
#4260 = ORIENTED_EDGE ( 'NONE', *, *, #9091, .F. ) ;
#4261 = CARTESIAN_POINT ( 'NONE',  ( 0.8323763977770604061, -4.658724279160015413, 10.37605171672202253 ) ) ;
#4262 = CARTESIAN_POINT ( 'NONE',  ( -15.00000000000000000, 19.99999999999999645, -5.999999999999999112 ) ) ;
#4263 = ORIENTED_EDGE ( 'NONE', *, *, #6696, .T. ) ;
#4264 = SURFACE_SIDE_STYLE ('',( #10113 ) ) ;
#4265 = EDGE_CURVE ( 'NONE', #467, #5853, #6071, .T. ) ;
#4266 = EDGE_LOOP ( 'NONE', ( #4433, #6896, #8282, #1953 ) ) ;
#4267 = LINE ( 'NONE', #8943, #6851 ) ;
#4268 = SURFACE_STYLE_FILL_AREA ( #9002 ) ;
#4269 = ORIENTED_EDGE ( 'NONE', *, *, #5645, .F. ) ;
#4270 =( BOUNDED_CURVE ( )  B_SPLINE_CURVE ( 2, ( #8175, #907, #116, #3340, #2287, #374, #6772, #1860, #1755, #9875, #4286, #9017, #1914, #2701, #6568, #10035, #8228, #6670, #1112, #4982, #7482, #3447, #2605, #2756, #2655, #2551, #7527, #9928, #5920, #5768, #1160, #5869, #5821, #3395, #960, #5034, #4387, #6624, #9074, #7633, #9819, #1808, #8280, #222, #6716, #9176, #9120, #4186, #1006, #5083, #8336, #4337, #4236, #1063, #272, #3499, #9976, #320, #7420, #5136, #163, #8382, #7577, #3546, #5971, #9225, #1965, #5187, #8434, #1465, #7991, #6278, #5293 ),
 .UNSPECIFIED., .F., .T. ) 
 B_SPLINE_CURVE_WITH_KNOTS ( ( 3, 2, 2, 2, 2, 2, 2, 2, 2, 2, 2, 2, 2, 2, 2, 2, 2, 2, 2, 2, 2, 2, 2, 2, 2, 2, 2, 2, 2, 2, 2, 2, 2, 2, 2, 2, 3 ),
 ( 0.000000000000000000, 0.02777777777777777624, 0.05555555555555555247, 0.08333333333333332871, 0.1111111111111111049, 0.1388888888888888951, 0.1666666666666666574, 0.1944444444444444475, 0.2222222222222222099, 0.2500000000000000000, 0.2777777777777777901, 0.3055555555555555802, 0.3333333333333333148, 0.3611111111111111049, 0.3888888888888888951, 0.4166666666666666852, 0.4444444444444444198, 0.4722222222222222099, 0.5000000000000000000, 0.5277777777777777901, 0.5555555555555555802, 0.5833333333333333703, 0.6111111111111111605, 0.6388888888888888395, 0.6666666666666666297, 0.6944444444444444198, 0.7222222222222222099, 0.7500000000000000000, 0.7777777777777777901, 0.8055555555555555802, 0.8333333333333333703, 0.8611111111111111605, 0.8888888888888888395, 0.9166666666666666297, 0.9444444444444444198, 0.9722222222222222099, 1.000000000000000000 ),
 .UNSPECIFIED. ) 
 CURVE ( )  GEOMETRIC_REPRESENTATION_ITEM ( )  RATIONAL_B_SPLINE_CURVE ( ( 1.000000000000000000, 0.8660254037844387076, 1.000000000000000000, 0.8660254037844387076, 1.000000000000000000, 0.8660254037844387076, 1.000000000000000000, 0.8660254037844387076, 1.000000000000000000, 0.8660254037844387076, 1.000000000000000000, 0.8660254037844387076, 1.000000000000000000, 0.8660254037844387076, 1.000000000000000000, 0.8660254037844387076, 1.000000000000000000, 0.8660254037844387076, 1.000000000000000000, 0.8660254037844387076, 1.000000000000000000, 0.8660254037844387076, 1.000000000000000000, 0.8660254037844387076, 1.000000000000000000, 0.8660254037844387076, 1.000000000000000000, 0.8660254037844387076, 1.000000000000000000, 0.8660254037844387076, 1.000000000000000000, 0.8660254037844387076, 1.000000000000000000, 0.8660254037844387076, 1.000000000000000000, 0.8660254037844387076, 1.000000000000000000, 0.8660254037844387076, 1.000000000000000000, 0.8660254037844387076, 1.000000000000000000, 0.8660254037844387076, 1.000000000000000000, 0.8660254037844387076, 1.000000000000000000, 0.8660254037844387076, 1.000000000000000000, 0.8660254037844387076, 1.000000000000000000, 0.8660254037844387076, 1.000000000000000000, 0.8660254037844387076, 1.000000000000000000, 0.8660254037844387076, 1.000000000000000000, 0.8660254037844387076, 1.000000000000000000, 0.8660254037844387076, 1.000000000000000000, 0.8660254037844387076, 1.000000000000000000, 0.8660254037844387076, 1.000000000000000000, 0.8660254037844387076, 1.000000000000000000, 0.8660254037844387076, 1.000000000000000000, 0.8660254037844387076, 1.000000000000000000, 0.8660254037844387076, 1.000000000000000000, 0.8660254037844387076, 1.000000000000000000 ) ) 
 REPRESENTATION_ITEM ( '' )  );
#4271 = CARTESIAN_POINT ( 'NONE',  ( 4.089228379062037178, -4.089228379062022967, 9.099999999999999645 ) ) ;
#4272 = CARTESIAN_POINT ( 'NONE',  ( 3.889087296526005488, 3.889087296526018811, 8.400000000000000355 ) ) ;
#4273 = CARTESIAN_POINT ( 'NONE',  ( -3.889087296526005044, -3.889087296526019255, 9.799999999999998934 ) ) ;
#4274 = ORIENTED_EDGE ( 'NONE', *, *, #5334, .T. ) ;
#4275 = CARTESIAN_POINT ( 'NONE',  ( 0.6146835312500001924, -11.93533689329915326, -0.1354166673494631989 ) ) ;
#4276 = AXIS2_PLACEMENT_3D ( 'NONE', #3914, #7140, #3118 ) ;
#4277 = EDGE_CURVE ( 'NONE', #4895, #7351, #6232, .T. ) ;
#4278 =( NAMED_UNIT ( * ) SI_UNIT ( $, .STERADIAN. ) SOLID_ANGLE_UNIT ( ) );
#4279 = EDGE_CURVE ( 'NONE', #1347, #4726, #1420, .T. ) ;
#4280 = VERTEX_POINT ( 'NONE', #680 ) ;
#4281 = FACE_OUTER_BOUND ( 'NONE', #8776, .T. ) ;
#4282 = FACE_OUTER_BOUND ( 'NONE', #311, .T. ) ;
#4283 = VERTEX_POINT ( 'NONE', #9598 ) ;
#4284 = CARTESIAN_POINT ( 'NONE',  ( 0.000000000000000000, -19.00000000000000711, 0.000000000000000000 ) ) ;
#4285 = VECTOR ( 'NONE', #5838, 1000.000000000000000 ) ;
#4286 = CARTESIAN_POINT ( 'NONE',  ( 0.6146835312499993043, -14.06466310670085562, -2.427083334016129967 ) ) ;
#4287 = CARTESIAN_POINT ( 'NONE',  ( -4.658724279160018078, 0.8323763977770419764, 12.02394828327797427 ) ) ;
#4288 = EDGE_LOOP ( 'NONE', ( #8053, #3580, #7927, #5963 ) ) ;
#4289 = CARTESIAN_POINT ( 'NONE',  ( 0.000000000000000000, -10.00000000000000000, -12.00000000000000000 ) ) ;
#4290 = CARTESIAN_POINT ( 'NONE',  ( -2.496947748567517333, 4.900535883036019058, 13.43999999999999950 ) ) ;
#4291 = ADVANCED_FACE ( 'NONE', ( #2325 ), #3069, .F. ) ;
#4292 = DIRECTION ( 'NONE',  ( -0.000000000000000000, -0.000000000000000000, -1.000000000000000000 ) ) ;
#4293 = CARTESIAN_POINT ( 'NONE',  ( -4.089228379062038066, 4.089228379062022078, 10.50000000000000000 ) ) ;
#4294 = CARTESIAN_POINT ( 'NONE',  ( 30.00000000000001066, 35.00000000000001421, -9.000000000000000000 ) ) ;
#4295 = DIRECTION ( 'NONE',  ( 0.000000000000000000, 0.000000000000000000, 1.000000000000000000 ) ) ;
#4296 = DIRECTION ( 'NONE',  ( -1.000000000000000000, 0.000000000000000000, -0.000000000000000000 ) ) ;
#4297 = CARTESIAN_POINT ( 'NONE',  ( 0.6162731882459174804, 4.458484982038668498, 6.316051716722022924 ) ) ;
#4298 = CARTESIAN_POINT ( 'NONE',  ( -1.229367062500000163, -13.00000000000000533, -1.968750000682796708 ) ) ;
#4299 = CARTESIAN_POINT ( 'NONE',  ( 4.860232935257354114, -2.576046737280751842, 2.363948283277975904 ) ) ;
#4300 = EDGE_CURVE ( 'NONE', #8225, #1785, #2272, .T. ) ;
#4301 = CARTESIAN_POINT ( 'NONE',  ( 1.229367062500000163, -12.29022459553277002, -2.677083334016129079 ) ) ;
#4302 = ORIENTED_EDGE ( 'NONE', *, *, #9033, .F. ) ;
#4303 = CARTESIAN_POINT ( 'NONE',  ( 4.940838830814703542, -2.417848759854246410, 7.156051716722023670 ) ) ;
#4304 = MECHANICAL_DESIGN_GEOMETRIC_PRESENTATION_REPRESENTATION (  '', ( #3974 ), #7361 ) ;
#4305 = DIRECTION ( 'NONE',  ( -1.000000000000000000, -0.000000000000000000, -0.000000000000000000 ) ) ;
#4306 = DIRECTION ( 'NONE',  ( -0.9396926207859105373, 0.3420201433256627732, 0.000000000000000000 ) ) ;
#4307 = VERTEX_POINT ( 'NONE', #6925 ) ;
#4308 = VECTOR ( 'NONE', #4434, 1000.000000000000000 ) ;
#4309 = CARTESIAN_POINT ( 'NONE',  ( 4.009529358847659708, -2.042957248827953709, 6.159999999999999254 ) ) ;
#4310 = AXIS2_PLACEMENT_3D ( 'NONE', #10027, #2799, #4432 ) ;
#4311 = CARTESIAN_POINT ( 'NONE',  ( 2.122056237541221524, -3.969226411068978777, 4.636051716722022320 ) ) ;
#4312 = CARTESIAN_POINT ( 'NONE',  ( 0.6146835312500001924, -11.93533689329915326, -2.760416667349463449 ) ) ;
#4313 = VERTEX_POINT ( 'NONE', #2167 ) ;
#4314 = AXIS2_PLACEMENT_3D ( 'NONE', #1417, #8734, #10450 ) ;
#4315 = VERTEX_POINT ( 'NONE', #5390 ) ;
#4316 = EDGE_CURVE ( 'NONE', #6690, #2207, #8298, .T. ) ;
#4317 = LINE ( 'NONE', #9517, #10436 ) ;
#4318 = CIRCLE ( 'NONE', #5674, 2.399999999999999911 ) ;
#4319 = CARTESIAN_POINT ( 'NONE',  ( 1.500000000000003775, -12.13397459621556962, -0.4583333333333337034 ) ) ;
#4320 = VERTEX_POINT ( 'NONE', #8790 ) ;
#4321 = CARTESIAN_POINT ( 'NONE',  ( 5.726445515403654873, -0.8124729078101852187, 1.416051716722023235 ) ) ;
#4322 = CARTESIAN_POINT ( 'NONE',  ( -2.625446233515515981, -5.152728359536500768, 1.259999999999999787 ) ) ;
#4323 = CARTESIAN_POINT ( 'NONE',  ( -5.711843387010018702, 0.9046671180729746187, 10.21999999999999709 ) ) ;
#4324 = ORIENTED_EDGE ( 'NONE', *, *, #343, .F. ) ;
#4325 = VECTOR ( 'NONE', #10295, 1000.000000000000000 ) ;
#4326 = CARTESIAN_POINT ( 'NONE',  ( 0.6146835312499993043, -14.06466310670085562, -0.3020833340161297453 ) ) ;
#4327 = ADVANCED_FACE ( 'NONE', ( #1533 ), #2912, .F. ) ;
#4328 = VECTOR ( 'NONE', #3866, 1000.000000000000000 ) ;
#4329 =( NAMED_UNIT ( * ) SI_UNIT ( $, .STERADIAN. ) SOLID_ANGLE_UNIT ( ) );
#4330 = VERTEX_POINT ( 'NONE', #6184 ) ;
#4331 =( BOUNDED_CURVE ( )  B_SPLINE_CURVE ( 2, ( #8720, #775, #7069, #6217, #10318, #3895, #5433 ),
 .UNSPECIFIED., .F., .F. ) 
 B_SPLINE_CURVE_WITH_KNOTS ( ( 3, 2, 2, 3 ),
 ( 0.000000000000000000, 0.02777777777777775195, 0.05555555555555550390, 0.08333333333333325932 ),
 .UNSPECIFIED. ) 
 CURVE ( )  GEOMETRIC_REPRESENTATION_ITEM ( )  RATIONAL_B_SPLINE_CURVE ( ( 1.000000000000000000, 0.8660254037844387076, 1.000000000000000000, 0.8660254037844387076, 1.000000000000000000, 0.8660254037844390407, 0.9999999999999996669 ) ) 
 REPRESENTATION_ITEM ( '' )  );
#4332 = CARTESIAN_POINT ( 'NONE',  ( -0.7500000000000007772, -14.29903810567666156, -2.666666666666666519 ) ) ;
#4333 = CARTESIAN_POINT ( 'NONE',  ( 10.00000000000000000, 5.241389472434725860, -4.711457988287000909 ) ) ;
#4334 = ORIENTED_EDGE ( 'NONE', *, *, #1635, .F. ) ;
#4335 = FACE_OUTER_BOUND ( 'NONE', #4369, .T. ) ;
#4336 = DIRECTION ( 'NONE',  ( 0.000000000000000000, -1.000000000000000000, -0.000000000000000000 ) ) ;
#4337 = CARTESIAN_POINT ( 'NONE',  ( 8.692241771943170539E-17, -11.58044919106553650, -0.7187500006827969301 ) ) ;
#4338 = CARTESIAN_POINT ( 'NONE',  ( 0.7916369971161419938, 4.430710083317576320, 12.72394828327797711 ) ) ;
#4339 = VERTEX_POINT ( 'NONE', #626 ) ;
#4340 = DIRECTION ( 'NONE',  ( 1.000000000000000000, 0.000000000000000000, 0.000000000000000000 ) ) ;
#4341 = ADVANCED_FACE ( 'NONE', ( #7139 ), #5341, .T. ) ;
#4342 = CARTESIAN_POINT ( 'NONE',  ( 5.152728359536493663, 2.625446233515533745, 11.33999999999999808 ) ) ;
#4343 = CARTESIAN_POINT ( 'NONE',  ( 10.00000000000000000, -6.200809695932771426, -0.7745709230445765314 ) ) ;
#4344 = CARTESIAN_POINT ( 'NONE',  ( -4.089228379062038066, 4.089228379062022078, 7.699999999999998401 ) ) ;
#4345 = DIRECTION ( 'NONE',  ( 0.000000000000000000, 0.000000000000000000, 1.000000000000000000 ) ) ;
#4346 = DIRECTION ( 'NONE',  ( 0.000000000000000000, 0.000000000000000000, 1.000000000000000000 ) ) ;
#4347 = DIRECTION ( 'NONE',  ( -0.000000000000000000, 1.000000000000000000, -0.000000000000000000 ) ) ;
#4348 = CARTESIAN_POINT ( 'NONE',  ( -4.009529358847660596, 2.042957248827953265, 1.959999999999999964 ) ) ;
#4349 = ADVANCED_FACE ( 'NONE', ( #1315 ), #9491, .F. ) ;
#4350 = EDGE_CURVE ( 'NONE', #946, #9203, #572, .T. ) ;
#4351 = CARTESIAN_POINT ( 'NONE',  ( 1.229367062500000385, -12.29022459553277002, -1.177083334016129967 ) ) ;
#4352 = CARTESIAN_POINT ( 'NONE',  ( -3.244753828200538148, -3.119207202478392116, 11.60394828327797434 ) ) ;
#4353 = CARTESIAN_POINT ( 'NONE',  ( -1.229367062500000163, -13.00000000000000533, -1.468750000682796486 ) ) ;
#4354 = ORIENTED_EDGE ( 'NONE', *, *, #2403, .T. ) ;
#4355 = CARTESIAN_POINT ( 'NONE',  ( 0.8603895577212593571, 5.432285873273261068, 13.71999999999999886 ) ) ;
#4356 = CARTESIAN_POINT ( 'NONE',  ( 3.586028019667255595, -7.750000000000000000, -12.00000000000000000 ) ) ;
#4357 = DIRECTION ( 'NONE',  ( -1.000000000000000000, -0.000000000000000000, -0.000000000000000000 ) ) ;
#4358 = VERTEX_POINT ( 'NONE', #10285 ) ;
#4359 = EDGE_CURVE ( 'NONE', #9494, #467, #1864, .T. ) ;
#4360 = CARTESIAN_POINT ( 'NONE',  ( 4.444597532678119300, 0.7039550926810472786, 5.879999999999999893 ) ) ;
#4361 = LINE ( 'NONE', #5210, #7274 ) ;
#4362 = CARTESIAN_POINT ( 'NONE',  ( 4.444597532678119300, 0.7039550926810472786, 3.079999999999999627 ) ) ;
#4363 = CARTESIAN_POINT ( 'NONE',  ( -0.6146835312500006365, -14.06466310670085562, -0.5104166673494635598 ) ) ;
#4364 = ORIENTED_EDGE ( 'NONE', *, *, #2586, .T. ) ;
#4365 = DIRECTION ( 'NONE',  ( 1.000000000000000000, 0.000000000000000000, 0.000000000000000000 ) ) ;
#4366 = EDGE_LOOP ( 'NONE', ( #4858, #5604, #2371, #3892, #9620, #4026 ) ) ;
#4367 = CARTESIAN_POINT ( 'NONE',  ( 27.00000000000001066, -25.00000000000000000, 0.000000000000000000 ) ) ;
#4368 = DIRECTION ( 'NONE',  ( 1.000000000000000000, -0.000000000000000000, -0.000000000000000000 ) ) ;
#4369 = EDGE_LOOP ( 'NONE', ( #2120, #9924 ) ) ;
#4370 = CARTESIAN_POINT ( 'NONE',  ( 2.625446233515515537, 5.152728359536502545, 13.85999999999999766 ) ) ;
#4371 = AXIS2_PLACEMENT_3D ( 'NONE', #9395, #6943, #8697 ) ;
#4372 = CARTESIAN_POINT ( 'NONE',  ( -0.9046671180729963790, 5.711843387010016926, 10.77999999999999936 ) ) ;
#4373 = CARTESIAN_POINT ( 'NONE',  ( -4.089228379062038066, 4.089228379062021190, 13.29999999999999538 ) ) ;
#4374 = ORIENTED_EDGE ( 'NONE', *, *, #1118, .F. ) ;
#4375 = CARTESIAN_POINT ( 'NONE',  ( 0.6146835312499993043, -14.06466310670085562, 0.1979166659838698661 ) ) ;
#4376 = ADVANCED_FACE ( 'NONE', ( #3856 ), #5413, .T. ) ;
#4377 = UNCERTAINTY_MEASURE_WITH_UNIT (LENGTH_MEASURE( 1.000000000000000082E-05 ), #8113, 'distance_accuracy_value', 'NONE');
#4378 = CIRCLE ( 'NONE', #2189, 4.000000000000000000 ) ;
#4379 = ORIENTED_EDGE ( 'NONE', *, *, #213, .T. ) ;
#4380 = DIRECTION ( 'NONE',  ( -1.000000000000000000, 0.000000000000000000, 0.000000000000000000 ) ) ;
#4381 = AXIS2_PLACEMENT_3D ( 'NONE', #6130, #4646, #9382 ) ;
#4382 = FACE_OUTER_BOUND ( 'NONE', #5666, .T. ) ;
#4383 = ORIENTED_EDGE ( 'NONE', *, *, #387, .T. ) ;
#4384 = DIRECTION ( 'NONE',  ( 0.3420201433256627732, -0.9396926207859105373, 0.000000000000000000 ) ) ;
#4385 = CLOSED_SHELL ( 'NONE', ( #5658, #3891, #2338, #4291, #6602, #4600, #3068, #1486, #9647 ) ) ;
#4386 = CARTESIAN_POINT ( 'NONE',  ( -2.000000000000000000, 0.000000000000000000, 0.000000000000000000 ) ) ;
#4387 = CARTESIAN_POINT ( 'NONE',  ( 1.229367062500000163, -13.00000000000000533, -1.343750000682796486 ) ) ;
#4388 = CARTESIAN_POINT ( 'NONE',  ( 0.7916369971161419938, 4.430710083317576320, 7.123948283277974802 ) ) ;
#4389 = ORIENTED_EDGE ( 'NONE', *, *, #5130, .F. ) ;
#4390 = VECTOR ( 'NONE', #2652, 1000.000000000000000 ) ;
#4391 = CARTESIAN_POINT ( 'NONE',  ( 0.000000000000000000, 0.000000000000000000, -14.00000000000000178 ) ) ;
#4392 = AXIS2_PLACEMENT_3D ( 'NONE', #9853, #1629, #6385 ) ;
#4393 = CARTESIAN_POINT ( 'NONE',  ( -0.8603895577212598011, -5.432285873273260179, 12.31999999999999851 ) ) ;
#4394 = CARTESIAN_POINT ( 'NONE',  ( 0.000000000000000000, 0.000000000000000000, -5.999999999999999112 ) ) ;
#4395 = CARTESIAN_POINT ( 'NONE',  ( 2.625446233515515093, 5.152728359536503433, 13.85999999999999943 ) ) ;
#4396 = AXIS2_PLACEMENT_3D ( 'NONE', #3219, #4758, #732 ) ;
#4397 = ADVANCED_FACE ( 'NONE', ( #4585 ), #9372, .F. ) ;
#4398 = PLANE ( 'NONE',  #9591 ) ;
#4399 = VECTOR ( 'NONE', #9448, 1000.000000000000000 ) ;
#4400 = CARTESIAN_POINT ( 'NONE',  ( 16.15239861966725599, -7.750000000000000000, -12.00000000000000000 ) ) ;
#4401 = DIRECTION ( 'NONE',  ( -1.000000000000000000, -0.000000000000000000, -0.000000000000000000 ) ) ;
#4402 = CARTESIAN_POINT ( 'NONE',  ( 2.064922774268895811, 4.258245684917319807, 12.05605171672202047 ) ) ;
#4403 = CIRCLE ( 'NONE', #7808, 1.249999999999993339 ) ;
#4404 = CARTESIAN_POINT ( 'NONE',  ( -0.7916369971161423269, -4.430710083317576320, 11.32394828327797676 ) ) ;
#4405 = CARTESIAN_POINT ( 'NONE',  ( 1.229367062500000163, -13.70977540446723886, -1.760416667349463227 ) ) ;
#4407 = VERTEX_POINT ( 'NONE', #7130 ) ;
#4406 = AXIS2_PLACEMENT_3D ( 'NONE', #963, #7637, #3450 ) ;
#4408 = EDGE_CURVE ( 'NONE', #9974, #6869, #7605, .T. ) ;
#4409 = CARTESIAN_POINT ( 'NONE',  ( 2.542276634908080535, 5.195105386651229118, 9.256051716722023315 ) ) ;
#4410 = EDGE_CURVE ( 'NONE', #9328, #3187, #5538, .T. ) ;
#4411 = VECTOR ( 'NONE', #8883, 1000.000000000000000 ) ;
#4412 = DIRECTION ( 'NONE',  ( 0.000000000000000000, 0.000000000000000000, 1.000000000000000000 ) ) ;
#4413 = PLANE ( 'NONE',  #2559 ) ;
#4414 = ORIENTED_EDGE ( 'NONE', *, *, #8007, .F. ) ;
#4415 = CARTESIAN_POINT ( 'NONE',  ( 4.215868657802586128, 2.148092372876346801, 11.33999999999999808 ) ) ;
#4416 = CARTESIAN_POINT ( 'NONE',  ( -9.000000000000000000, 19.99999999999999645, 15.00000000000000000 ) ) ;
#4417 = CARTESIAN_POINT ( 'NONE',  ( 2.042957248827968808, -4.009529358847652603, 0.8399999999999999689 ) ) ;
#4418 = CARTESIAN_POINT ( 'NONE',  ( -2.607672531582950546E-16, -14.41955080893447416, 0.03124999931720332663 ) ) ;
#4419 = EDGE_LOOP ( 'NONE', ( #1035, #7285 ) ) ;
#4420 = ADVANCED_FACE ( 'NONE', ( #9535 ), #10385, .F. ) ;
#4421 =( LENGTH_UNIT ( ) NAMED_UNIT ( * ) SI_UNIT ( .MILLI., .METRE. ) );
#4422 = VERTEX_POINT ( 'NONE', #6279 ) ;
#4423 = CARTESIAN_POINT ( 'NONE',  ( 0.000000000000000000, -7.063614741696270016, 8.843061888689529582 ) ) ;
#4424 = DIRECTION ( 'NONE',  ( 0.000000000000000000, 1.000000000000000000, 0.000000000000000000 ) ) ;
#4425 = LINE ( 'NONE', #8419, #7622 ) ;
#4426 = VERTEX_POINT ( 'NONE', #10276 ) ;
#4427 = CARTESIAN_POINT ( 'NONE',  ( -5.711843387010018702, 0.9046671180729746187, 13.01999999999999424 ) ) ;
#4428 = CARTESIAN_POINT ( 'NONE',  ( -5.711843387010018702, 0.9046671180729746187, 13.01999999999999424 ) ) ;
#4429 = CARTESIAN_POINT ( 'NONE',  ( -4.900535883036028828, 2.496947748567499126, 7.559999999999998721 ) ) ;
#4430 = ORIENTED_EDGE ( 'NONE', *, *, #9523, .T. ) ;
#4431 = CARTESIAN_POINT ( 'NONE',  ( 3.000000000000002665, 0.000000000000000000, 0.000000000000000000 ) ) ;
#4432 = DIRECTION ( 'NONE',  ( 1.000000000000000000, 0.000000000000000000, 0.000000000000000000 ) ) ;
#4433 = ORIENTED_EDGE ( 'NONE', *, *, #1957, .T. ) ;
#4434 = DIRECTION ( 'NONE',  ( 0.3420201433256627732, -0.9396926207859105373, 0.000000000000000000 ) ) ;
#4435 = MANIFOLD_SOLID_BREP ( 'M3 Clearance Hole2', #3883 ) ;
#4436 = DIRECTION ( 'NONE',  ( 0.000000000000000000, 1.000000000000000000, 0.000000000000000000 ) ) ;
#4437 = ORIENTED_EDGE ( 'NONE', *, *, #9033, .T. ) ;
#4438 = CARTESIAN_POINT ( 'NONE',  ( 4.000000000000000888, -7.673322273190750664, 3.656518192455050276 ) ) ;
#4439 = DIRECTION ( 'NONE',  ( 0.000000000000000000, -0.000000000000000000, 1.000000000000000000 ) ) ;
#4440 = CARTESIAN_POINT ( 'NONE',  ( 25.00000000000000000, -4.000000000000000000, -2.000000000000000000 ) ) ;
#4441 = CARTESIAN_POINT ( 'NONE',  ( -3.279728542977953687, 3.411736077305369541, 9.503948283277974696 ) ) ;
#4442 = VERTEX_POINT ( 'NONE', #6120 ) ;
#4443 = LINE ( 'NONE', #7692, #10191 ) ;
#4444 = VECTOR ( 'NONE', #4863, 1000.000000000000000 ) ;
#4445 = CYLINDRICAL_SURFACE ( 'NONE', #2431, 3.000000000000000000 ) ;
#4446 = ADVANCED_FACE ( 'NONE', ( #6330 ), #1521, .T. ) ;
#4447 = CARTESIAN_POINT ( 'NONE',  ( 1.070288219556879694, -11.94905607805280567, 1.518836458664385706E-16 ) ) ;
#4448 = CARTESIAN_POINT ( 'NONE',  ( -2.000000000000000000, 7.003298780661491918, -4.817032923780498521 ) ) ;
#4449 = CARTESIAN_POINT ( 'NONE',  ( 11.29375735928344504, -10.02539999999999942, -12.00000000000000000 ) ) ;
#4450 = EDGE_CURVE ( 'NONE', #4315, #8225, #507, .T. ) ;
#4451 = DIRECTION ( 'NONE',  ( 0.000000000000000000, -1.000000000000000000, 0.000000000000000000 ) ) ;
#4452 = DIRECTION ( 'NONE',  ( 0.000000000000000000, 0.000000000000000000, 1.000000000000000000 ) ) ;
#4453 = CARTESIAN_POINT ( 'NONE',  ( 0.6162731882459174804, 4.458484982038668498, 14.71605171672202239 ) ) ;
#4454 = CARTESIAN_POINT ( 'NONE',  ( 1.229367062499999719, -13.70977540446724063, -0.7604166673494633377 ) ) ;
#4455 = EDGE_CURVE ( 'NONE', #2545, #8537, #9138, .T. ) ;
#4456 = CARTESIAN_POINT ( 'NONE',  ( -5.446173322633801384, -0.7727076532861678615, 3.483948283277976898 ) ) ;
#4457 =( GEOMETRIC_REPRESENTATION_CONTEXT ( 3 ) GLOBAL_UNCERTAINTY_ASSIGNED_CONTEXT ( ( #4485 ) ) GLOBAL_UNIT_ASSIGNED_CONTEXT ( ( #2386, #3177, #3862 ) ) REPRESENTATION_CONTEXT ( 'NONE', 'WORKASPACE' ) );
#4458 = CARTESIAN_POINT ( 'NONE',  ( 1.229367062500000163, -13.70977540446723886, 0.2395833326505366900 ) ) ;
#4459 = ORIENTED_EDGE ( 'NONE', *, *, #9528, .F. ) ;
#4460 = CARTESIAN_POINT ( 'NONE',  ( 0.000000000000000000, 0.000000000000000000, 0.000000000000000000 ) ) ;
#4461 = DIRECTION ( 'NONE',  ( 0.000000000000000000, -0.000000000000000000, 1.000000000000000000 ) ) ;
#4462 = CARTESIAN_POINT ( 'NONE',  ( 0.000000000000000000, 0.000000000000000000, -17.00000000000000000 ) ) ;
#4463 = PLANE ( 'NONE',  #4080 ) ;
#4464 = EDGE_LOOP ( 'NONE', ( #6695, #9053, #5028, #4263 ) ) ;
#4465 = VECTOR ( 'NONE', #5655, 1000.000000000000000 ) ;
#4466 = CARTESIAN_POINT ( 'NONE',  ( -4.009529358847660596, 2.042957248827953265, 10.35999999999999943 ) ) ;
#4467 = DIRECTION ( 'NONE',  ( 1.000000000000000000, 0.000000000000000000, 0.000000000000000000 ) ) ;
#4468 = EDGE_CURVE ( 'NONE', #4238, #1944, #723, .T. ) ;
#4469 = EDGE_CURVE ( 'NONE', #10319, #4238, #2900, .T. ) ;
#4470 = CARTESIAN_POINT ( 'NONE',  ( 2.042957248827968808, -4.009529358847652603, 6.439999999999999503 ) ) ;
#4471 = CARTESIAN_POINT ( 'NONE',  ( 1.500000000000000444, -12.13397459621556607, -2.958333333333333037 ) ) ;
#4472 =( GEOMETRIC_REPRESENTATION_CONTEXT ( 3 ) GLOBAL_UNCERTAINTY_ASSIGNED_CONTEXT ( ( #8527 ) ) GLOBAL_UNIT_ASSIGNED_CONTEXT ( ( #8220, #8262, #832 ) ) REPRESENTATION_CONTEXT ( 'NONE', 'WORKASPACE' ) );
#4473 = ORIENTED_EDGE ( 'NONE', *, *, #9019, .T. ) ;
#4474 = ORIENTED_EDGE ( 'NONE', *, *, #4782, .F. ) ;
#4475 = FACE_OUTER_BOUND ( 'NONE', #4511, .T. ) ;
#4476 = DIRECTION ( 'NONE',  ( -0.000000000000000000, -0.000000000000000000, -1.000000000000000000 ) ) ;
#4477 = DIRECTION ( 'NONE',  ( -1.000000000000000000, -4.625929269271485914E-16, 0.000000000000000000 ) ) ;
#4478 = ORIENTED_EDGE ( 'NONE', *, *, #8174, .F. ) ;
#4479 = CARTESIAN_POINT ( 'NONE',  ( -0.9968613283357868893, 5.697241258616382531, 6.176051716722023244 ) ) ;
#4480 = CARTESIAN_POINT ( 'NONE',  ( 5.711843387010018702, -0.9046671180729751738, 8.820000000000000284 ) ) ;
#4481 = CARTESIAN_POINT ( 'NONE',  ( -0.9046671180729963790, 5.711843387010016926, 10.77999999999999936 ) ) ;
#4482 = ORIENTED_EDGE ( 'NONE', *, *, #996, .F. ) ;
#4483 = EDGE_CURVE ( 'NONE', #9543, #3690, #6970, .T. ) ;
#4484 = CARTESIAN_POINT ( 'NONE',  ( 5.999999999999999112, 26.99999999999999289, 3.000000000000000000 ) ) ;
#4485 = UNCERTAINTY_MEASURE_WITH_UNIT (LENGTH_MEASURE( 1.000000000000000082E-05 ), #2386, 'distance_accuracy_value', 'NONE');
#4486 = AXIS2_PLACEMENT_3D ( 'NONE', #254, #7303, #3481 ) ;
#4487 = VERTEX_POINT ( 'NONE', #7073 ) ;
#4488 = DIRECTION ( 'NONE',  ( 1.000000000000000000, -0.000000000000000000, -0.000000000000000000 ) ) ;
#4489 = MANIFOLD_SOLID_BREP ( 'Boss-Extrude1', #6268 ) ;
#4490 = CARTESIAN_POINT ( 'NONE',  ( -2.000000000000000000, 5.793104693147763662, 2.343061888689530026 ) ) ;
#4491 = VERTEX_POINT ( 'NONE', #826 ) ;
#4492 = CYLINDRICAL_SURFACE ( 'NONE', #7951, 6.248999999999999666 ) ;
#4493 = VECTOR ( 'NONE', #4884, 1000.000000000000000 ) ;
#4494 = LINE ( 'NONE', #574, #5818 ) ;
#4495 = CARTESIAN_POINT ( 'NONE',  ( -3.244753828200538148, -3.119207202478392116, 8.803948283277977183 ) ) ;
#4496 = ORIENTED_EDGE ( 'NONE', *, *, #353, .F. ) ;
#4497 = EDGE_CURVE ( 'NONE', #4339, #5618, #9487, .T. ) ;
#4498 = VECTOR ( 'NONE', #1819, 1000.000000000000000 ) ;
#4499 = CARTESIAN_POINT ( 'NONE',  ( 30.00000000000001066, 1.959434878635756602E-16, 1.599999999999992983 ) ) ;
#4500 = CARTESIAN_POINT ( 'NONE',  ( 0.000000000000000000, 6.000000000000000000, -12.00000000000000000 ) ) ;
#4501 = CARTESIAN_POINT ( 'NONE',  ( 1.300000000000000044, 1.478016689125442484, -1.626303258728256651E-15 ) ) ;
#4502 = CARTESIAN_POINT ( 'NONE',  ( -26.99999999999998934, 0.000000000000000000, 1.599999999999998979 ) ) ;
#4503 = DIRECTION ( 'NONE',  ( -1.000000000000000000, -0.000000000000000000, -0.000000000000000000 ) ) ;
#4504 = CARTESIAN_POINT ( 'NONE',  ( -15.00000000000000000, 19.99999999999999645, -9.000000000000000000 ) ) ;
#4505 = CARTESIAN_POINT ( 'NONE',  ( -2.000000000000024425, 15.00000000000000355, -5.999999999999999112 ) ) ;
#4506 = CARTESIAN_POINT ( 'NONE',  ( 2.500000000000007105, -28.99999999999999289, 0.000000000000000000 ) ) ;
#4507 = CARTESIAN_POINT ( 'NONE',  ( 4.444597532678119300, 0.7039550926810472786, 0.2799999999999999711 ) ) ;
#4508 = CARTESIAN_POINT ( 'NONE',  ( -1.229367062500000385, -13.70977540446723886, -0.4270833340161298564 ) ) ;
#4509 = CARTESIAN_POINT ( 'NONE',  ( 4.458484982038663169, 0.6162731882459350219, 10.48394828327797512 ) ) ;
#4510 = CARTESIAN_POINT ( 'NONE',  ( 1.229367062500000163, -12.29022459553277002, -1.177083334016129967 ) ) ;
#4511 = EDGE_LOOP ( 'NONE', ( #4700, #772, #1733, #1141 ) ) ;
#4512 = CARTESIAN_POINT ( 'NONE',  ( 10.00000000000000000, 0.000000000000000000, 0.000000000000000000 ) ) ;
#4513 = CARTESIAN_POINT ( 'NONE',  ( 0.000000000000000000, 1.478016689125442484, -1.626303258728256651E-15 ) ) ;
#4514 = CARTESIAN_POINT ( 'NONE',  ( -29.99999999999998934, -35.00000000000000000, -9.000000000000000000 ) ) ;
#4515 = EDGE_CURVE ( 'NONE', #1597, #6552, #9699, .T. ) ;
#4516 = CARTESIAN_POINT ( 'NONE',  ( 11.00000000000000355, 1.665213485140613626E-16, -1.219500000000000028 ) ) ;
#4517 = PRODUCT ( 'main housing', 'main housing', '', ( #3087 ) ) ;
#4518 = ORIENTED_EDGE ( 'NONE', *, *, #5300, .F. ) ;
#4519 = DIRECTION ( 'NONE',  ( 0.000000000000000000, 0.000000000000000000, -1.000000000000000000 ) ) ;
#4520 = CARTESIAN_POINT ( 'NONE',  ( 4.000000000000000888, -7.673322273190701814, -3.656518192455153748 ) ) ;
#4521 = CARTESIAN_POINT ( 'NONE',  ( -4.673326407553653361, 0.7401821875142517992, 1.819999999999999396 ) ) ;
#4522 = CARTESIAN_POINT ( 'NONE',  ( -2.607672531582950546E-16, -14.41955080893447416, -1.968750000682796708 ) ) ;
#4523 = EDGE_LOOP ( 'NONE', ( #3501, #2758, #1483, #3725 ) ) ;
#4524 = ORIENTED_EDGE ( 'NONE', *, *, #9504, .T. ) ;
#4525 = FACE_OUTER_BOUND ( 'NONE', #3262, .T. ) ;
#4526 = EDGE_CURVE ( 'NONE', #3111, #5332, #3954, .T. ) ;
#4527 = PLANE ( 'NONE',  #6601 ) ;
#4528 = VERTEX_POINT ( 'NONE', #7348 ) ;
#4529 = CARTESIAN_POINT ( 'NONE',  ( -0.7727076532861475444, -5.446173322633804048, 10.51605171672202133 ) ) ;
#4530 = FILL_AREA_STYLE_COLOUR ( '', #3379 ) ;
#4531 = ORIENTED_EDGE ( 'NONE', *, *, #748, .T. ) ;
#4532 = DIRECTION ( 'NONE',  ( 1.000000000000000000, 0.000000000000000000, 0.000000000000000000 ) ) ;
#4533 = EDGE_LOOP ( 'NONE', ( #6599, #5263, #6529, #776 ) ) ;
#4534 = EDGE_LOOP ( 'NONE', ( #2471, #7142, #1359, #7756 ) ) ;
#4535 = EDGE_CURVE ( 'NONE', #8939, #7393, #8153, .T. ) ;
#4536 = DIRECTION ( 'NONE',  ( 0.000000000000000000, -0.000000000000000000, 1.000000000000000000 ) ) ;
#4537 = EDGE_CURVE ( 'NONE', #244, #10205, #140, .T. ) ;
#4538 = FACE_OUTER_BOUND ( 'NONE', #2598, .T. ) ;
#4539 = EDGE_LOOP ( 'NONE', ( #7448, #1669, #888, #6649, #6810 ) ) ;
#4540 = CARTESIAN_POINT ( 'NONE',  ( 13.82973899676619745, -10.00000000000000000, -12.00000000000000000 ) ) ;
#4541 = FACE_OUTER_BOUND ( 'NONE', #10257, .T. ) ;
#4542 = CARTESIAN_POINT ( 'NONE',  ( 5.446173322633801384, 0.7727076532861675284, 2.083948283277976543 ) ) ;
#4543 = ORIENTED_EDGE ( 'NONE', *, *, #9279, .T. ) ;
#4544 = LINE ( 'NONE', #477, #7803 ) ;
#4545 = VECTOR ( 'NONE', #8, 1000.000000000000000 ) ;
#4546 = FACE_BOUND ( 'NONE', #2951, .T. ) ;
#4547 = DIRECTION ( 'NONE',  ( 1.000000000000000000, 0.000000000000000000, 0.000000000000000000 ) ) ;
#4548 = VECTOR ( 'NONE', #6769, 1000.000000000000000 ) ;
#4549 = EDGE_CURVE ( 'NONE', #8074, #5539, #8808, .T. ) ;
#4550 = CARTESIAN_POINT ( 'NONE',  ( 3.889087296526005488, 3.889087296526018811, 13.99999999999999822 ) ) ;
#4551 = CLOSED_SHELL ( 'NONE', ( #9403, #642, #4154, #4376 ) ) ;
#4552 = DIRECTION ( 'NONE',  ( -1.000000000000000000, -0.000000000000000000, 0.000000000000000000 ) ) ;
#4553 = PLANE ( 'NONE',  #7386 ) ;
#4554 = LINE ( 'NONE', #3761, #1975 ) ;
#4555 = DIRECTION ( 'NONE',  ( 0.3420201433256627732, -0.9396926207859105373, 0.000000000000000000 ) ) ;
#4556 = CARTESIAN_POINT ( 'NONE',  ( 3.119207202478379681, 3.244753828200549695, 12.19605171672202282 ) ) ;
#4557 = MECHANICAL_DESIGN_GEOMETRIC_PRESENTATION_REPRESENTATION (  '', ( #3720 ), #5076 ) ;
#4558 = CARTESIAN_POINT ( 'NONE',  ( 1.229367062499999719, -13.70977540446724063, 0.2395833326505366900 ) ) ;
#4559 = CARTESIAN_POINT ( 'NONE',  ( 2.417848759854264618, -4.940838830814695548, 11.04394828327797562 ) ) ;
#4560 = CARTESIAN_POINT ( 'NONE',  ( 17.57694265928344635, -10.02539999999999942, -12.00000000000000000 ) ) ;
#4561 = ORIENTED_EDGE ( 'NONE', *, *, #5229, .F. ) ;
#4562 = CIRCLE ( 'NONE', #11, 8.500000000000000000 ) ;
#4563 = LINE ( 'NONE', #6152, #8816 ) ;
#4564 = CARTESIAN_POINT ( 'NONE',  ( 0.000000000000000000, -10.00000000000000000, 0.000000000000000000 ) ) ;
#4565 = LINE ( 'NONE', #8506, #3150 ) ;
#4566 = LINE ( 'NONE', #5416, #5418 ) ;
#4567 = PRODUCT_DEFINITION ( 'UNKNOWN', '', #6508, #9375 ) ;
#4568 = VERTEX_POINT ( 'NONE', #10495 ) ;
#4569 = MECHANICAL_DESIGN_GEOMETRIC_PRESENTATION_REPRESENTATION (  '', ( #4235 ), #1187 ) ;
#4570 = CARTESIAN_POINT ( 'NONE',  ( 19.29399126966725575, -7.750000000000000000, -12.00000000000000000 ) ) ;
#4571 = SURFACE_SIDE_STYLE ('',( #5421 ) ) ;
#4572 = CARTESIAN_POINT ( 'NONE',  ( -3.345732310141667831, 3.345732310141653620, 4.900000000000000355 ) ) ;
#4573 = AXIS2_PLACEMENT_3D ( 'NONE', #4101, #8979, #4947 ) ;
#4574 = CARTESIAN_POINT ( 'NONE',  ( 0.6146835312500001924, -11.93533689329915326, -1.760416667349463449 ) ) ;
#4575 = ORIENTED_EDGE ( 'NONE', *, *, #4867, .T. ) ;
#4576 = AXIS2_PLACEMENT_3D ( 'NONE', #1749, #9716, #745 ) ;
#4577 = VECTOR ( 'NONE', #9461, 1000.000000000000000 ) ;
#4578 = ORIENTED_EDGE ( 'NONE', *, *, #9352, .T. ) ;
#4579 = DIRECTION ( 'NONE',  ( 0.3420201433256627732, -0.9396926207859105373, 0.000000000000000000 ) ) ;
#4580 = AXIS2_PLACEMENT_3D ( 'NONE', #6224, #9318, #1208 ) ;
#4581 = DIRECTION ( 'NONE',  ( 0.8660254037844397068, 0.000000000000000000, -0.4999999999999983347 ) ) ;
#4582 = VERTEX_POINT ( 'NONE', #9640 ) ;
#4583 = CARTESIAN_POINT ( 'NONE',  ( -4.940838830814703542, 2.417848759854245078, 11.35605171672202296 ) ) ;
#4584 = CIRCLE ( 'NONE', #4090, 1.280000000000000027 ) ;
#4585 = FACE_OUTER_BOUND ( 'NONE', #5910, .T. ) ;
#4586 = ORIENTED_EDGE ( 'NONE', *, *, #2218, .T. ) ;
#4587 = CARTESIAN_POINT ( 'NONE',  ( 1.500000000000000222, -13.00000000000000533, -1.500000000000000000 ) ) ;
#4588 = EDGE_CURVE ( 'NONE', #5003, #4330, #7240, .T. ) ;
#4589 = ORIENTED_EDGE ( 'NONE', *, *, #328, .F. ) ;
#4590 = ORIENTED_EDGE ( 'NONE', *, *, #2673, .T. ) ;
#4591 = DIRECTION ( 'NONE',  ( -1.000000000000000000, 0.000000000000000000, 0.000000000000000000 ) ) ;
#4592 = FACE_OUTER_BOUND ( 'NONE', #1994, .T. ) ;
#4593 = ORIENTED_EDGE ( 'NONE', *, *, #7981, .F. ) ;
#4594 = CARTESIAN_POINT ( 'NONE',  ( -9.000000000000000000, 19.99999999999999645, 15.00000000000000000 ) ) ;
#4595 = DIRECTION ( 'NONE',  ( -1.000000000000000000, 0.000000000000000000, 0.000000000000000000 ) ) ;
#4596 = CARTESIAN_POINT ( 'NONE',  ( -5.697241258616385196, 0.9968613283357647958, 3.623948283277976135 ) ) ;
#4597 = VERTEX_POINT ( 'NONE', #5012 ) ;
#4598 = LINE ( 'NONE', #7898, #3229 ) ;
#4599 = EDGE_CURVE ( 'NONE', #5555, #6919, #4852, .T. ) ;
#4600 = ADVANCED_FACE ( 'NONE', ( #3366, #9047 ), #4957, .T. ) ;
#4601 = DIRECTION ( 'NONE',  ( 0.000000000000000000, 0.000000000000000000, 1.000000000000000000 ) ) ;
#4602 = DIRECTION ( 'NONE',  ( 1.000000000000000000, 0.000000000000000000, 0.000000000000000000 ) ) ;
#4603 = ADVANCED_BREP_SHAPE_REPRESENTATION ( '', ( #4735, #2101 ), #4472 ) ;
#4604 = CARTESIAN_POINT ( 'NONE',  ( -3.181725716174720991E-16, -14.73205080756888563, -0.1250000000000001110 ) ) ;
#4605 = CARTESIAN_POINT ( 'NONE',  ( 13.01080596966725622, -7.750000000000000000, -12.00000000000000000 ) ) ;
#4606 = PLANE ( 'NONE',  #1799 ) ;
#4607 = LINE ( 'NONE', #7849, #9771 ) ;
#4608 = CARTESIAN_POINT ( 'NONE',  ( 8.152164709283445276, -10.02539999999999942, -12.00000000000000000 ) ) ;
#4609 = CARTESIAN_POINT ( 'NONE',  ( -4.009529358847660596, 2.042957248827953265, 4.759999999999999787 ) ) ;
#4610 = CARTESIAN_POINT ( 'NONE',  ( 8.692241771943169307E-17, -11.58044919106553294, -2.218750000682796486 ) ) ;
#4611 = ADVANCED_FACE ( 'NONE', ( #41 ), #2478, .T. ) ;
#4612 = CARTESIAN_POINT ( 'NONE',  ( 4.023224611898322145, -4.155232146225737111, 10.90394828327797327 ) ) ;
#4613 = FACE_OUTER_BOUND ( 'NONE', #7290, .T. ) ;
#4614 = VERTEX_POINT ( 'NONE', #8097 ) ;
#4615 = CIRCLE ( 'NONE', #6990, 8.500000000000000000 ) ;
#4616 = CARTESIAN_POINT ( 'NONE',  ( -6.000000000000011546, 33.55452559259863676, 1.999999999999995337 ) ) ;
#4617 = CARTESIAN_POINT ( 'NONE',  ( 1.300000000000000044, -1.108512516844082141, -0.6399999999999991251 ) ) ;
#4618 = CARTESIAN_POINT ( 'NONE',  ( 8.980342580332745683, -7.750000000000000000, -12.00000000000000000 ) ) ;
#4619 = DIRECTION ( 'NONE',  ( 1.000000000000000000, -0.000000000000000000, 0.000000000000000000 ) ) ;
#4620 = CARTESIAN_POINT ( 'NONE',  ( 1.500000000000000222, -13.00000000000000533, -3.000000000000000000 ) ) ;
#4621 = EDGE_LOOP ( 'NONE', ( #7059, #1773, #6177, #9877 ) ) ;
#4622 = VECTOR ( 'NONE', #15, 1000.000000000000000 ) ;
#4623 = ADVANCED_FACE ( 'NONE', ( #4904, #1577, #887 ), #6594, .F. ) ;
#4624 = CARTESIAN_POINT ( 'NONE',  ( -4.215868657802586128, -2.148092372876348133, 7.139999999999997016 ) ) ;
#4625 = CARTESIAN_POINT ( 'NONE',  ( 1.500000000000000222, -13.00000000000000533, 0.000000000000000000 ) ) ;
#4626 = ORIENTED_EDGE ( 'NONE', *, *, #7509, .F. ) ;
#4627 = ORIENTED_EDGE ( 'NONE', *, *, #6480, .F. ) ;
#4628 = VECTOR ( 'NONE', #1378, 1000.000000000000000 ) ;
#4629 = DIRECTION ( 'NONE',  ( 0.000000000000000000, 0.000000000000000000, -1.000000000000000000 ) ) ;
#4630 = CARTESIAN_POINT ( 'NONE',  ( -10.00000000000000000, 0.000000000000000000, 0.000000000000000000 ) ) ;
#4631 = ORIENTED_EDGE ( 'NONE', *, *, #2671, .F. ) ;
#4632 = CARTESIAN_POINT ( 'NONE',  ( -0.7727076532861475444, -5.446173322633804048, 13.31605171672202204 ) ) ;
#4633 = CARTESIAN_POINT ( 'NONE',  ( 1.300000000000000044, 1.108512516844080364, -0.6400000000000017897 ) ) ;
#4634 = CARTESIAN_POINT ( 'NONE',  ( 3.889087296526005488, 3.889087296526018811, 13.99999999999999822 ) ) ;
#4635 = ORIENTED_EDGE ( 'NONE', *, *, #985, .F. ) ;
#4636 = DIRECTION ( 'NONE',  ( 0.000000000000000000, 1.000000000000000000, 0.000000000000000000 ) ) ;
#4637 = STYLED_ITEM ( 'NONE', ( #8940 ), #8917 ) ;
#4638 = CARTESIAN_POINT ( 'NONE',  ( 0.9968613283357860011, -5.697241258616382531, 10.37605171672202253 ) ) ;
#4639 = ORIENTED_EDGE ( 'NONE', *, *, #8731, .T. ) ;
#4640 = EDGE_CURVE ( 'NONE', #3105, #6166, #8935, .T. ) ;
#4641 = ORIENTED_EDGE ( 'NONE', *, *, #3871, .T. ) ;
#4642 = DIRECTION ( 'NONE',  ( 0.000000000000000000, -1.000000000000000000, 0.000000000000000000 ) ) ;
#4643 = DIRECTION ( 'NONE',  ( 0.000000000000000000, 0.000000000000000000, -1.000000000000000000 ) ) ;
#4644 = CARTESIAN_POINT ( 'NONE',  ( -26.99999999999998934, -35.00000000000000000, -6.000000000000000000 ) ) ;
#4645 = ORIENTED_EDGE ( 'NONE', *, *, #7937, .F. ) ;
#4646 = DIRECTION ( 'NONE',  ( 1.000000000000000000, 0.000000000000000000, 0.000000000000000000 ) ) ;
#4647 = EDGE_CURVE ( 'NONE', #2213, #6828, #4361, .T. ) ;
#4648 = DIRECTION ( 'NONE',  ( 0.9396926207859105373, -0.3420201433256627732, 0.000000000000000000 ) ) ;
#4649 = CARTESIAN_POINT ( 'NONE',  ( -0.9480714621563718358, -5.418398423912716311, 5.723948283277976223 ) ) ;
#4650 = ORIENTED_EDGE ( 'NONE', *, *, #3463, .T. ) ;
#4651 = VECTOR ( 'NONE', #4380, 1000.000000000000000 ) ;
#4652 = DIRECTION ( 'NONE',  ( 1.000000000000000000, -0.000000000000000000, -0.000000000000000000 ) ) ;
#4653 = DIRECTION ( 'NONE',  ( -1.000000000000000000, -0.000000000000000000, 0.000000000000000000 ) ) ;
#4654 = DIRECTION ( 'NONE',  ( -1.000000000000000000, -0.000000000000000000, -0.000000000000000000 ) ) ;
#4655 = CARTESIAN_POINT ( 'NONE',  ( 16.98057649071655817, 6.025400000000000311, -12.00000000000000000 ) ) ;
#4656 = AXIS2_PLACEMENT_3D ( 'NONE', #4367, #6808, #8516 ) ;
#4657 = CARTESIAN_POINT ( 'NONE',  ( 0.000000000000000000, -13.00000000000000533, -3.000000000000000000 ) ) ;
#4658 = CARTESIAN_POINT ( 'NONE',  ( 19.29399126966725575, -7.750000000000000000, -12.00000000000000000 ) ) ;
#4659 = AXIS2_PLACEMENT_3D ( 'NONE', #869, #9886, #8242 ) ;
#4660 = CARTESIAN_POINT ( 'NONE',  ( 1.300000000000000044, 0.000000000000000000, 0.000000000000000000 ) ) ;
#4661 = CARTESIAN_POINT ( 'NONE',  ( 4.215868657802586128, 2.148092372876346801, 8.539999999999999147 ) ) ;
#4662 = CARTESIAN_POINT ( 'NONE',  ( 1.229367062500000385, -12.29022459553277002, -2.802083334016129523 ) ) ;
#4663 = AXIS2_PLACEMENT_3D ( 'NONE', #6991, #1382, #9503 ) ;
#4664 = CARTESIAN_POINT ( 'NONE',  ( 0.9480714621563713917, 5.418398423912717199, 12.72394828327797711 ) ) ;
#4665 = CARTESIAN_POINT ( 'NONE',  ( 8.000000000000001776, 0.005878491403557128264, -7.047692205288322853 ) ) ;
#4666 = CIRCLE ( 'NONE', #9423, 0.1499999999999999667 ) ;
#4667 = ORIENTED_EDGE ( 'NONE', *, *, #567, .T. ) ;
#4668 = SHAPE_DEFINITION_REPRESENTATION ( #10389, #7608 ) ;
#4669 = CARTESIAN_POINT ( 'NONE',  ( 7.555798540716556211, -10.02539999999999942, 0.000000000000000000 ) ) ;
#4670 = CARTESIAN_POINT ( 'NONE',  ( -0.7500000000000007772, -14.29903810567666156, -0.6666666666666669627 ) ) ;
#4671 = ADVANCED_FACE ( 'NONE', ( #1138 ), #9301, .T. ) ;
#4672 = CARTESIAN_POINT ( 'NONE',  ( 1.500000000000000222, -13.00000000000000533, -0.5000000000000000000 ) ) ;
#4673 = DIRECTION ( 'NONE',  ( 0.000000000000000000, 0.000000000000000000, -1.000000000000000000 ) ) ;
#4674 = EDGE_CURVE ( 'NONE', #8221, #2939, #8457, .T. ) ;
#4675 = CARTESIAN_POINT ( 'NONE',  ( -9.000000000000000000, 19.99999999999999645, 13.00000000000000000 ) ) ;
#4676 = ORIENTED_EDGE ( 'NONE', *, *, #9166, .T. ) ;
#4677 = CARTESIAN_POINT ( 'NONE',  ( 13.82973899676619745, 6.000000000000000000, -12.00000000000000000 ) ) ;
#4678 = CARTESIAN_POINT ( 'NONE',  ( 10.00000000000000000, 1.106368468154538931, -8.427689411260562480 ) ) ;
#4679 = CARTESIAN_POINT ( 'NONE',  ( 3.181980515339458471, 3.181980515339470461, 11.19999999999999751 ) ) ;
#4680 = CARTESIAN_POINT ( 'NONE',  ( 1.500000000000000222, -13.00000000000000533, -0.5000000000000000000 ) ) ;
#4681 = ORIENTED_EDGE ( 'NONE', *, *, #9432, .F. ) ;
#4682 = EDGE_LOOP ( 'NONE', ( #7052, #1423 ) ) ;
#4683 = EDGE_CURVE ( 'NONE', #1470, #8741, #6756, .T. ) ;
#4684 = CARTESIAN_POINT ( 'NONE',  ( 1.530808498934188612E-16, -19.00000000000000711, 1.249999999999997558 ) ) ;
#4685 = CARTESIAN_POINT ( 'NONE',  ( -2.000000000000000000, 1.418488851014483076, -6.085876303339363247 ) ) ;
#4686 = VERTEX_POINT ( 'NONE', #5111 ) ;
#4687 = CARTESIAN_POINT ( 'NONE',  ( 5.726445515403654873, -0.8124729078101852187, 7.016051716722022213 ) ) ;
#4688 = LINE ( 'NONE', #2014, #3368 ) ;
#4689 = DIRECTION ( 'NONE',  ( 0.000000000000000000, 0.000000000000000000, -1.000000000000000000 ) ) ;
#4690 = VERTEX_POINT ( 'NONE', #7451 ) ;
#4691 = DIRECTION ( 'NONE',  ( 0.000000000000000000, 0.000000000000000000, 1.000000000000000000 ) ) ;
#4692 = CARTESIAN_POINT ( 'NONE',  ( 2.542276634908080535, 5.195105386651229118, 12.05605171672202047 ) ) ;
#4693 = ORIENTED_EDGE ( 'NONE', *, *, #6417, .F. ) ;
#4694 = CARTESIAN_POINT ( 'NONE',  ( 21.54671318033274829, 3.750000000000000000, 0.000000000000000000 ) ) ;
#4695 = LINE ( 'NONE', #2433, #7960 ) ;
#4696 = EDGE_LOOP ( 'NONE', ( #2945, #1526, #793, #3733 ) ) ;
#4697 = CARTESIAN_POINT ( 'NONE',  ( 3.586028019667255595, 3.750000000000000000, 0.000000000000000000 ) ) ;
#4698 = CARTESIAN_POINT ( 'NONE',  ( 0.4444353696672553311, 3.750000000000000000, 0.000000000000000000 ) ) ;
#4699 = CARTESIAN_POINT ( 'NONE',  ( 4.860232935257354114, -2.576046737280751842, 2.363948283277975904 ) ) ;
#4700 = ORIENTED_EDGE ( 'NONE', *, *, #6153, .F. ) ;
#4701 = CARTESIAN_POINT ( 'NONE',  ( 0.7499999999999991118, -14.29903810567666333, -1.645833334698926675 ) ) ;
#4702 = LINE ( 'NONE', #2123, #2094 ) ;
#4703 = FILL_AREA_STYLE ('',( #8745 ) ) ;
#4704 = ORIENTED_EDGE ( 'NONE', *, *, #5130, .T. ) ;
#4705 = FACE_OUTER_BOUND ( 'NONE', #5856, .T. ) ;
#4706 = DIRECTION ( 'NONE',  ( -0.000000000000000000, -1.000000000000000000, -0.000000000000000000 ) ) ;
#4707 = CYLINDRICAL_SURFACE ( 'NONE', #8467, 1.500000000000000222 ) ;
#4708 = DIRECTION ( 'NONE',  ( -2.312964634635742957E-16, 1.000000000000000000, 0.000000000000000000 ) ) ;
#4709 =( REPRESENTATION_RELATIONSHIP ('NONE','NONE', #5100, #8347 ) REPRESENTATION_RELATIONSHIP_WITH_TRANSFORMATION ( #5622 )SHAPE_REPRESENTATION_RELATIONSHIP( ) );
#4710 = CARTESIAN_POINT ( 'NONE',  ( 18.40512053033274853, -7.750000000000000000, -12.00000000000000000 ) ) ;
#4711 = CARTESIAN_POINT ( 'NONE',  ( 0.7039550926810297371, 4.444597532678122853, 5.319999999999999396 ) ) ;
#4712 = MANIFOLD_SOLID_BREP ( 'Boss-Extrude2', #4385 ) ;
#4713 = AXIS2_PLACEMENT_3D ( 'NONE', #3081, #6091, #2025 ) ;
#4714 = CARTESIAN_POINT ( 'NONE',  ( 1.229367062499999719, -13.70977540446724063, -1.385416667349463671 ) ) ;
#4715 = CARTESIAN_POINT ( 'NONE',  ( 2.417848759854264618, -4.940838830814695548, 5.443948283277975975 ) ) ;
#4716 = DIRECTION ( 'NONE',  ( 0.000000000000000000, 0.000000000000000000, 1.000000000000000000 ) ) ;
#4717 = EDGE_CURVE ( 'NONE', #5181, #837, #2375, .T. ) ;
#4718 = VERTEX_POINT ( 'NONE', #7658 ) ;
#4719 = APPLICATION_PROTOCOL_DEFINITION ( 'draft international standard', 'automotive_design', 1998, #5988 ) ;
#4720 = CARTESIAN_POINT ( 'NONE',  ( -0.8603895577212598011, -5.432285873273260179, 1.119999999999999885 ) ) ;
#4721 = CIRCLE ( 'NONE', #4217, 2.000000000000000000 ) ;
#4722 = DIRECTION ( 'NONE',  ( -0.000000000000000000, -0.000000000000000000, -1.000000000000000000 ) ) ;
#4723 = ORIENTED_EDGE ( 'NONE', *, *, #4782, .T. ) ;
#4724 = AXIS2_PLACEMENT_3D ( 'NONE', #8173, #1752, #4131 ) ;
#4725 = CARTESIAN_POINT ( 'NONE',  ( 1.530808498934188612E-16, 18.99999999999999289, -1.249999999999997558 ) ) ;
#4726 = VERTEX_POINT ( 'NONE', #9098 ) ;
#4727 = CARTESIAN_POINT ( 'NONE',  ( 25.00000000000000000, -4.000000000000000000, -10.00000000000000000 ) ) ;
#4728 = DIRECTION ( 'NONE',  ( -1.000000000000000000, -0.000000000000000000, 0.000000000000000000 ) ) ;
#4729 = AXIS2_PLACEMENT_3D ( 'NONE', #8629, #1312, #7835 ) ;
#4730 = CARTESIAN_POINT ( 'NONE',  ( 3.181980515339458471, 3.181980515339470461, 8.400000000000000355 ) ) ;
#4731 = PRODUCT_DEFINITION_CONTEXT ( 'detailed design', #9259, 'design' ) ;
#4732 = EDGE_CURVE ( 'NONE', #8579, #4568, #246, .T. ) ;
#4733 = VECTOR ( 'NONE', #1409, 1000.000000000000000 ) ;
#4734 = CARTESIAN_POINT ( 'NONE',  ( -3.181725716174720498E-16, -14.73205080756888385, -0.6250000000000001110 ) ) ;
#4735 = MANIFOLD_SOLID_BREP ( 'M3 Tapped Hole2', #7609 ) ;
#4736 = EDGE_CURVE ( 'NONE', #3797, #4252, #9200, .T. ) ;
#4737 = ORIENTED_EDGE ( 'NONE', *, *, #3034, .T. ) ;
#4738 =( BOUNDED_CURVE ( )  B_SPLINE_CURVE ( 2, ( #3309, #4301, #3465, #1824, #879, #4251, #1668, #6689, #4893, #8350, #5103, #9945, #1079, #7547, #3514, #7338, #1231, #3615, #6149, #3769, #10099, #5151, #1131, #4405, #389, #2873, #6999, #489, #10251, #8401, #4353, #1330, #5359, #1983, #5203, #5938, #7593, #4510, #6950, #6793, #9292, #543, #2032, #6842, #6099, #9349, #7755, #9244, #9191, #3717, #8449, #10204, #3565, #1930, #1178, #6039, #8500, #336, #5261, #9401, #1284, #2138, #7811, #10049, #2773, #2825, #2083, #5310, #5986, #7651, #8599, #4458, #2930 ),
 .UNSPECIFIED., .F., .F. ) 
 B_SPLINE_CURVE_WITH_KNOTS ( ( 3, 2, 2, 2, 2, 2, 2, 2, 2, 2, 2, 2, 2, 2, 2, 2, 2, 2, 2, 2, 2, 2, 2, 2, 2, 2, 2, 2, 2, 2, 2, 2, 2, 2, 2, 2, 3 ),
 ( 0.000000000000000000, 0.02777777777777777624, 0.05555555555555555247, 0.08333333333333332871, 0.1111111111111111049, 0.1388888888888888951, 0.1666666666666666574, 0.1944444444444444475, 0.2222222222222222099, 0.2500000000000000000, 0.2777777777777777901, 0.3055555555555555802, 0.3333333333333333148, 0.3611111111111111049, 0.3888888888888888951, 0.4166666666666666852, 0.4444444444444444198, 0.4722222222222222099, 0.5000000000000000000, 0.5277777777777777901, 0.5555555555555555802, 0.5833333333333333703, 0.6111111111111111605, 0.6388888888888888395, 0.6666666666666666297, 0.6944444444444444198, 0.7222222222222222099, 0.7500000000000000000, 0.7777777777777777901, 0.8055555555555555802, 0.8333333333333333703, 0.8611111111111111605, 0.8888888888888888395, 0.9166666666666666297, 0.9444444444444444198, 0.9722222222222222099, 1.000000000000000000 ),
 .UNSPECIFIED. ) 
 CURVE ( )  GEOMETRIC_REPRESENTATION_ITEM ( )  RATIONAL_B_SPLINE_CURVE ( ( 1.000000000000000000, 0.8660254037844387076, 1.000000000000000000, 0.8660254037844387076, 1.000000000000000000, 0.8660254037844387076, 1.000000000000000000, 0.8660254037844387076, 1.000000000000000000, 0.8660254037844387076, 1.000000000000000000, 0.8660254037844387076, 1.000000000000000000, 0.8660254037844387076, 1.000000000000000000, 0.8660254037844387076, 1.000000000000000000, 0.8660254037844387076, 1.000000000000000000, 0.8660254037844387076, 1.000000000000000000, 0.8660254037844387076, 1.000000000000000000, 0.8660254037844387076, 1.000000000000000000, 0.8660254037844387076, 1.000000000000000000, 0.8660254037844387076, 1.000000000000000000, 0.8660254037844387076, 1.000000000000000000, 0.8660254037844387076, 1.000000000000000000, 0.8660254037844387076, 1.000000000000000000, 0.8660254037844387076, 1.000000000000000000, 0.8660254037844387076, 1.000000000000000000, 0.8660254037844387076, 1.000000000000000000, 0.8660254037844387076, 1.000000000000000000, 0.8660254037844387076, 1.000000000000000000, 0.8660254037844387076, 1.000000000000000000, 0.8660254037844387076, 1.000000000000000000, 0.8660254037844387076, 1.000000000000000000, 0.8660254037844387076, 1.000000000000000000, 0.8660254037844387076, 1.000000000000000000, 0.8660254037844387076, 1.000000000000000000, 0.8660254037844387076, 1.000000000000000000, 0.8660254037844387076, 1.000000000000000000, 0.8660254037844387076, 1.000000000000000000, 0.8660254037844387076, 1.000000000000000000, 0.8660254037844387076, 1.000000000000000000, 0.8660254037844387076, 1.000000000000000000, 0.8660254037844387076, 1.000000000000000000, 0.8660254037844387076, 1.000000000000000000 ) ) 
 REPRESENTATION_ITEM ( '' )  );
#4739 = ORIENTED_EDGE ( 'NONE', *, *, #8678, .F. ) ;
#4740 = CARTESIAN_POINT ( 'NONE',  ( -2.499999999999992895, -28.99999999999999289, 3.061616997868383634E-16 ) ) ;
#4741 = VECTOR ( 'NONE', #4477, 1000.000000000000000 ) ;
#4742 = CARTESIAN_POINT ( 'NONE',  ( 1.300000000000000044, 0.7390083445627193548, -1.280000000000000693 ) ) ;
#4743 = ORIENTED_EDGE ( 'NONE', *, *, #2185, .F. ) ;
#4744 = VECTOR ( 'NONE', #2994, 1000.000000000000000 ) ;
#4745 = PLANE ( 'NONE',  #5059 ) ;
#4746 = AXIS2_PLACEMENT_3D ( 'NONE', #4391, #1812, #4340 ) ;
#4747 = EDGE_LOOP ( 'NONE', ( #3271, #10167, #10210, #6129 ) ) ;
#4748 = DIRECTION ( 'NONE',  ( 0.000000000000000000, 0.000000000000000000, 1.000000000000000000 ) ) ;
#4749 = CARTESIAN_POINT ( 'NONE',  ( 0.8323763977770604061, -4.658724279160015413, 1.976051716722022844 ) ) ;
#4750 = AXIS2_PLACEMENT_3D ( 'NONE', #10218, #7723, #2102 ) ;
#4751 = EDGE_CURVE ( 'NONE', #216, #1449, #7453, .T. ) ;
#4752 = VECTOR ( 'NONE', #137, 1000.000000000000000 ) ;
#4753 = ORIENTED_EDGE ( 'NONE', *, *, #1500, .F. ) ;
#4754 = ORIENTED_EDGE ( 'NONE', *, *, #4178, .F. ) ;
#4755 = VECTOR ( 'NONE', #1654, 1000.000000000000000 ) ;
#4756 = CARTESIAN_POINT ( 'NONE',  ( 1.300000000000000044, 0.7390083445627224634, 1.279999999999999138 ) ) ;
#4757 = EDGE_CURVE ( 'NONE', #6915, #2636, #9465, .T. ) ;
#4758 = DIRECTION ( 'NONE',  ( 1.000000000000000000, 0.000000000000000000, 0.000000000000000000 ) ) ;
#4759 = AXIS2_PLACEMENT_3D ( 'NONE', #773, #612, #3840 ) ;
#4760 = EDGE_LOOP ( 'NONE', ( #9513, #5036, #3961, #8318 ) ) ;
#4761 = DIRECTION ( 'NONE',  ( -1.000000000000000000, -0.000000000000000000, -0.000000000000000000 ) ) ;
#4762 = CARTESIAN_POINT ( 'NONE',  ( 7.546553696766196140, -10.00000000000000000, -12.00000000000000000 ) ) ;
#4763 = CARTESIAN_POINT ( 'NONE',  ( -2.708615832122950096, -5.110351332421780413, 0.2639482832779765920 ) ) ;
#4764 = EDGE_LOOP ( 'NONE', ( #10009, #2594, #418, #5791, #6261 ) ) ;
#4765 = CARTESIAN_POINT ( 'NONE',  ( 1.229367062499999719, -13.70977540446724063, -2.260416667349463005 ) ) ;
#4766 = PLANE ( 'NONE',  #9377 ) ;
#4767 = ORIENTED_EDGE ( 'NONE', *, *, #8967, .T. ) ;
#4768 = DIRECTION ( 'NONE',  ( -1.000000000000000000, 0.000000000000000000, 0.000000000000000000 ) ) ;
#4769 = LINE ( 'NONE', #2600, #8823 ) ;
#4770 = CYLINDRICAL_SURFACE ( 'NONE', #3550, 2.000000000000001776 ) ;
#4771 = LINE ( 'NONE', #10466, #5178 ) ;
#4772 = CARTESIAN_POINT ( 'NONE',  ( 22.43558391966725907, 3.750000000000000000, -12.00000000000000000 ) ) ;
#4773 = CARTESIAN_POINT ( 'NONE',  ( -4.673326407553653361, 0.7401821875142517992, 4.620000000000000107 ) ) ;
#4774 = ORIENTED_EDGE ( 'NONE', *, *, #5513, .F. ) ;
#4775 = MANIFOLD_SOLID_BREP ( 'Thread1', #7956 ) ;
#4776 = DIRECTION ( 'NONE',  ( 0.000000000000000000, 0.000000000000000000, -1.000000000000000000 ) ) ;
#4777 = EDGE_CURVE ( 'NONE', #1449, #6865, #3677, .T. ) ;
#4778 = CARTESIAN_POINT ( 'NONE',  ( 5.697241258616385196, -0.9968613283357656840, 7.823948283277974980 ) ) ;
#4779 = PLANE ( 'NONE',  #1754 ) ;
#4780 = ORIENTED_EDGE ( 'NONE', *, *, #253, .F. ) ;
#4781 = SHAPE_DEFINITION_REPRESENTATION ( #1484, #7954 ) ;
#4782 = EDGE_CURVE ( 'NONE', #2528, #3281, #1398, .T. ) ;
#4783 = CARTESIAN_POINT ( 'NONE',  ( 4.000000000000000888, -8.497168642645966941, 0.2193742428684610779 ) ) ;
#4784 = DIRECTION ( 'NONE',  ( 0.000000000000000000, 0.000000000000000000, -1.000000000000000000 ) ) ;
#4785 = ORIENTED_EDGE ( 'NONE', *, *, #3034, .F. ) ;
#4786 = PLANE ( 'NONE',  #3656 ) ;
#4787 = CARTESIAN_POINT ( 'NONE',  ( 16.98057649071655817, 6.025400000000000311, -12.00000000000000000 ) ) ;
#4788 = PRODUCT_DEFINITION_SHAPE ( 'NONE', 'NONE',  #5214 ) ;
#4789 = CARTESIAN_POINT ( 'NONE',  ( 0.000000000000000000, -13.00000000000000533, 2.000000000000000000 ) ) ;
#4790 = ADVANCED_FACE ( 'NONE', ( #8664 ), #9524, .T. ) ;
#4791 = DIRECTION ( 'NONE',  ( 0.000000000000000000, 0.000000000000000000, 1.000000000000000000 ) ) ;
#4792 = CARTESIAN_POINT ( 'NONE',  ( 4.215868657802586128, 2.148092372876346801, 11.33999999999999808 ) ) ;
#4793 = VECTOR ( 'NONE', #5497, 1000.000000000000000 ) ;
#4794 = CARTESIAN_POINT ( 'NONE',  ( 0.7499999999999991118, -14.29903810567666333, -1.083333333333333481 ) ) ;
#4795 = ORIENTED_EDGE ( 'NONE', *, *, #5697, .F. ) ;
#4796 = EDGE_LOOP ( 'NONE', ( #8780, #8050, #1233, #250 ) ) ;
#4797 = DIRECTION ( 'NONE',  ( 0.000000000000000000, 0.000000000000000000, 1.000000000000000000 ) ) ;
#4798 = VECTOR ( 'NONE', #8206, 1000.000000000000000 ) ;
#4799 = CYLINDRICAL_SURFACE ( 'NONE', #5586, 8.500000000000000000 ) ;
#4800 = VERTEX_POINT ( 'NONE', #5318 ) ;
#4801 = DIRECTION ( 'NONE',  ( 0.000000000000000000, 0.000000000000000000, 1.000000000000000000 ) ) ;
#4802 = EDGE_CURVE ( 'NONE', #7195, #4215, #6960, .T. ) ;
#4803 = ORIENTED_EDGE ( 'NONE', *, *, #1956, .F. ) ;
#4804 = CARTESIAN_POINT ( 'NONE',  ( -4.940838830814703542, 2.417848759854245078, 14.15605171672202012 ) ) ;
#4805 = EDGE_LOOP ( 'NONE', ( #3311, #497, #6112, #7712 ) ) ;
#4806 = VECTOR ( 'NONE', #6240, 1000.000000000000000 ) ;
#4807 = DIRECTION ( 'NONE',  ( -1.000000000000000000, 0.000000000000000000, 0.000000000000000000 ) ) ;
#4808 = LINE ( 'NONE', #47, #3216 ) ;
#4809 = EDGE_LOOP ( 'NONE', ( #5547, #718, #6124, #7469 ) ) ;
#4810 = EDGE_CURVE ( 'NONE', #4950, #1471, #10213, .T. ) ;
#4811 = CARTESIAN_POINT ( 'NONE',  ( 3.889087296526005488, 3.889087296526018811, 8.400000000000000355 ) ) ;
#4812 = EDGE_CURVE ( 'NONE', #9748, #7999, #8510, .T. ) ;
#4813 = CARTESIAN_POINT ( 'NONE',  ( 0.000000000000000000, 6.000000000000000000, -12.00000000000000000 ) ) ;
#4814 = CARTESIAN_POINT ( 'NONE',  ( -0.8603895577212598011, -5.432285873273260179, 1.119999999999999885 ) ) ;
#4816 = ORIENTED_EDGE ( 'NONE', *, *, #414, .T. ) ;
#4815 = AXIS2_PLACEMENT_3D ( 'NONE', #7739, #4648, #6131 ) ;
#4817 = CARTESIAN_POINT ( 'NONE',  ( -0.7499999999999997780, -11.70096189432334555, 0.1041666653010730748 ) ) ;
#4818 =( GEOMETRIC_REPRESENTATION_CONTEXT ( 3 ) GLOBAL_UNCERTAINTY_ASSIGNED_CONTEXT ( ( #7282 ) ) GLOBAL_UNIT_ASSIGNED_CONTEXT ( ( #1906, #3492, #4329 ) ) REPRESENTATION_CONTEXT ( 'NONE', 'WORKASPACE' ) );
#4819 = ORIENTED_EDGE ( 'NONE', *, *, #9980, .T. ) ;
#4820 = LINE ( 'NONE', #6401, #7009 ) ;
#4821 = DIRECTION ( 'NONE',  ( 0.000000000000000000, -0.000000000000000000, -1.000000000000000000 ) ) ;
#4822 = CARTESIAN_POINT ( 'NONE',  ( 19.29399126966725575, -7.750000000000000000, 0.000000000000000000 ) ) ;
#4823 = ADVANCED_FACE ( 'NONE', ( #3834 ), #7061, .F. ) ;
#4824 = LINE ( 'NONE', #3237, #8742 ) ;
#4825 = DIRECTION ( 'NONE',  ( 0.000000000000000000, 0.000000000000000000, -1.000000000000000000 ) ) ;
#4826 = CARTESIAN_POINT ( 'NONE',  ( 4.009529358847659708, -2.042957248827953709, 8.959999999999999076 ) ) ;
#4827 = VERTEX_POINT ( 'NONE', #6264 ) ;
#4828 = CARTESIAN_POINT ( 'NONE',  ( -2.607672531582950546E-16, -14.41955080893447416, 0.03124999931720332663 ) ) ;
#4829 = VECTOR ( 'NONE', #9560, 1000.000000000000000 ) ;
#4830 = CARTESIAN_POINT ( 'NONE',  ( 0.9046671180729951578, -5.711843387010016926, 3.779999999999998472 ) ) ;
#4831 = CARTESIAN_POINT ( 'NONE',  ( 16.15239861966725599, 3.750000000000000000, -12.00000000000000000 ) ) ;
#4832 = VECTOR ( 'NONE', #7782, 1000.000000000000000 ) ;
#4833 = DIRECTION ( 'NONE',  ( 1.000000000000000000, -0.000000000000000000, -0.000000000000000000 ) ) ;
#4834 = AXIS2_PLACEMENT_3D ( 'NONE', #5415, #8660, #7165 ) ;
#4835 = CARTESIAN_POINT ( 'NONE',  ( -2.000000000000000000, -7.673322273190701814, -3.656518192455153748 ) ) ;
#4836 = CARTESIAN_POINT ( 'NONE',  ( 1.070288219556879694, -11.94905607805280567, 1.518836458664385706E-16 ) ) ;
#4837 = LINE ( 'NONE', #74, #9510 ) ;
#4838 = CARTESIAN_POINT ( 'NONE',  ( -5.999999999999999112, 26.99999999999999289, -4.000000000000000000 ) ) ;
#4839 = VECTOR ( 'NONE', #6471, 1000.000000000000000 ) ;
#4840 = CARTESIAN_POINT ( 'NONE',  ( 0.000000000000000000, 0.000000000000000000, 3.000000000000000000 ) ) ;
#4841 = CARTESIAN_POINT ( 'NONE',  ( 10.00000000000000000, 0.000000000000000000, 0.000000000000000000 ) ) ;
#4842 = AXIS2_PLACEMENT_3D ( 'NONE', #1489, #10354, #7152 ) ;
#4843 = CARTESIAN_POINT ( 'NONE',  ( -4.009529358847660596, 2.042957248827953265, 10.35999999999999943 ) ) ;
#4844 = UNCERTAINTY_MEASURE_WITH_UNIT (LENGTH_MEASURE( 1.000000000000000082E-05 ), #7026, 'distance_accuracy_value', 'NONE');
#4845 = CARTESIAN_POINT ( 'NONE',  ( -3.181725716174720498E-16, -14.73205080756888385, -0.1250000000000001110 ) ) ;
#4846 = ORIENTED_EDGE ( 'NONE', *, *, #8389, .F. ) ;
#4847 = ORIENTED_EDGE ( 'NONE', *, *, #7915, .T. ) ;
#4848 = CARTESIAN_POINT ( 'NONE',  ( 27.00000000000001066, 35.00000000000001421, 9.000000000000000000 ) ) ;
#4849 = DIRECTION ( 'NONE',  ( -1.000000000000000000, -1.156482317317871478E-16, 0.000000000000000000 ) ) ;
#4850 = ORIENTED_EDGE ( 'NONE', *, *, #3799, .T. ) ;
#4851 = CARTESIAN_POINT ( 'NONE',  ( -4.673326407553653361, 0.7401821875142517992, 1.819999999999999618 ) ) ;
#4852 = LINE ( 'NONE', #2523, #2706 ) ;
#4853 = VERTEX_POINT ( 'NONE', #4678 ) ;
#4854 = CARTESIAN_POINT ( 'NONE',  ( 0.7727076532861471003, 5.446173322633805824, 11.91605171672202346 ) ) ;
#4855 = ORIENTED_EDGE ( 'NONE', *, *, #5996, .T. ) ;
#4856 = SHAPE_REPRESENTATION_RELATIONSHIP ( 'NONE' , 'NONE' ,  #9732, #8917 ) ;
#4857 = EDGE_CURVE ( 'NONE', #4426, #2398, #9413, .T. ) ;
#4858 = ORIENTED_EDGE ( 'NONE', *, *, #2171, .T. ) ;
#4859 = DIRECTION ( 'NONE',  ( 0.000000000000000000, 0.000000000000000000, 1.000000000000000000 ) ) ;
#4860 = CARTESIAN_POINT ( 'NONE',  ( 1.500000000000000222, -13.00000000000000533, -2.000000000000000000 ) ) ;
#4861 = VERTEX_POINT ( 'NONE', #10263 ) ;
#4862 = CARTESIAN_POINT ( 'NONE',  ( -5.152728359536494551, -2.625446233515535077, 7.139999999999997016 ) ) ;
#4863 = DIRECTION ( 'NONE',  ( -0.000000000000000000, -0.000000000000000000, -1.000000000000000000 ) ) ;
#4864 = CARTESIAN_POINT ( 'NONE',  ( 2.496947748567516889, -4.900535883036019946, 0.8399999999999999689 ) ) ;
#4865 = ORIENTED_EDGE ( 'NONE', *, *, #2733, .F. ) ;
#4866 = CARTESIAN_POINT ( 'NONE',  ( -0.7499999999999997780, -11.70096189432334555, -0.8958333346989268975 ) ) ;
#4867 = EDGE_CURVE ( 'NONE', #6026, #6209, #5368, .T. ) ;
#4868 = SURFACE_STYLE_USAGE ( .BOTH. , #5705 ) ;
#4869 = EDGE_CURVE ( 'NONE', #6398, #1737, #2713, .T. ) ;
#4870 = ORIENTED_EDGE ( 'NONE', *, *, #3547, .F. ) ;
#4871 = PRODUCT_DEFINITION_SHAPE ( 'NONE', 'NONE',  #3931 ) ;
#4872 = LINE ( 'NONE', #9815, #1946 ) ;
#4873 = CARTESIAN_POINT ( 'NONE',  ( 27.00000000000001066, -25.00000000000000000, -1.999999999999997780 ) ) ;
#4874 = CARTESIAN_POINT ( 'NONE',  ( 0.000000000000000000, 0.000000000000000000, -4.000000000000000000 ) ) ;
#4875 = CARTESIAN_POINT ( 'NONE',  ( 10.00000000000000000, 4.438567988583180579, -7.249076783337634389 ) ) ;
#4876 = DIRECTION ( 'NONE',  ( 0.000000000000000000, -0.4999999999999992784, 0.8660254037844390407 ) ) ;
#4877 = CARTESIAN_POINT ( 'NONE',  ( 4.658724279160018966, -0.8323763977770426425, 5.023948283277976046 ) ) ;
#4878 = EDGE_LOOP ( 'NONE', ( #6710, #6755, #9644, #6646, #9151, #2524, #10217, #1367 ) ) ;
#4879 = CARTESIAN_POINT ( 'NONE',  ( 1.229367062499999719, -13.70977540446724063, -0.3854166673494633932 ) ) ;
#4880 = CARTESIAN_POINT ( 'NONE',  ( 2.625446233515515537, 5.152728359536502545, 8.259999999999999787 ) ) ;
#4881 = EDGE_CURVE ( 'NONE', #3335, #3788, #3885, .T. ) ;
#4882 = DIRECTION ( 'NONE',  ( 0.000000000000000000, 0.000000000000000000, 1.000000000000000000 ) ) ;
#4883 = FACE_OUTER_BOUND ( 'NONE', #9299, .T. ) ;
#4884 = DIRECTION ( 'NONE',  ( 0.3420201433256627732, 0.9396926207859105373, -0.000000000000000000 ) ) ;
#4885 = DIRECTION ( 'NONE',  ( -1.000000000000000000, -0.000000000000000000, -0.000000000000000000 ) ) ;
#4886 = VECTOR ( 'NONE', #2237, 1000.000000000000000 ) ;
#4887 = CARTESIAN_POINT ( 'NONE',  ( -29.99999999999998934, 0.000000000000000000, 0.000000000000000000 ) ) ;
#4888 = VERTEX_POINT ( 'NONE', #7280 ) ;
#4889 = CARTESIAN_POINT ( 'NONE',  ( 0.7727076532861471003, 5.446173322633805824, 14.71605171672202239 ) ) ;
#4890 = CARTESIAN_POINT ( 'NONE',  ( 9.000000000000000000, 19.99999999999999645, 15.00000000000000000 ) ) ;
#4891 = CARTESIAN_POINT ( 'NONE',  ( -2.000000000000001776, 0.000000000000000000, 0.000000000000000000 ) ) ;
#4892 = CARTESIAN_POINT ( 'NONE',  ( -0.7916369971161423269, -4.430710083317576320, 2.923948283277976401 ) ) ;
#4893 = CARTESIAN_POINT ( 'NONE',  ( -0.6146835312500006365, -14.06466310670085562, -2.385416667349463005 ) ) ;
#4894 = AXIS2_PLACEMENT_3D ( 'NONE', #3778, #2993, #3727 ) ;
#4895 = VERTEX_POINT ( 'NONE', #2355 ) ;
#4896 = CIRCLE ( 'NONE', #7442, 1.599999999999986766 ) ;
#4897 = ORIENTED_EDGE ( 'NONE', *, *, #6153, .T. ) ;
#4898 = PRODUCT_RELATED_PRODUCT_CATEGORY ( 'part', '', ( #8677 ) ) ;
#4899 = CARTESIAN_POINT ( 'NONE',  ( 0.000000000000000000, -0.7390083445627200209, 1.280000000000001137 ) ) ;
#4900 = CARTESIAN_POINT ( 'NONE',  ( 1.999999999999975797, 15.00000000000000355, -6.000000000000009770 ) ) ;
#4901 = ORIENTED_EDGE ( 'NONE', *, *, #6017, .F. ) ;
#4902 = VECTOR ( 'NONE', #6621, 1000.000000000000000 ) ;
#4903 = CARTESIAN_POINT ( 'NONE',  ( 2.042957248827968808, -4.009529358847652603, 0.8399999999999999689 ) ) ;
#4904 = FACE_BOUND ( 'NONE', #8942, .T. ) ;
#4905 = VERTEX_POINT ( 'NONE', #8085 ) ;
#4906 =( GEOMETRIC_REPRESENTATION_CONTEXT ( 3 ) GLOBAL_UNCERTAINTY_ASSIGNED_CONTEXT ( ( #8982 ) ) GLOBAL_UNIT_ASSIGNED_CONTEXT ( ( #1784, #3267, #7398 ) ) REPRESENTATION_CONTEXT ( 'NONE', 'WORKASPACE' ) );
#4907 = CARTESIAN_POINT ( 'NONE',  ( -4.049832306626335310, 1.963858260114700327, 8.556051716722022249 ) ) ;
#4908 = EDGE_CURVE ( 'NONE', #3971, #4105, #1665, .T. ) ;
#4909 = ORIENTED_EDGE ( 'NONE', *, *, #8588, .F. ) ;
#4910 = EDGE_LOOP ( 'NONE', ( #881, #476 ) ) ;
#4911 = EDGE_CURVE ( 'NONE', #6440, #6214, #816, .T. ) ;
#4912 = CARTESIAN_POINT ( 'NONE',  ( -4.000000000000000000, -13.00000000000000533, 2.000000000000000000 ) ) ;
#4913 = VECTOR ( 'NONE', #4728, 1000.000000000000000 ) ;
#4914 = CARTESIAN_POINT ( 'NONE',  ( 0.000000000000000000, 3.275930187719169848E-16, -2.600000000000000089 ) ) ;
#4915 = ORIENTED_EDGE ( 'NONE', *, *, #3838, .F. ) ;
#4916 = CARTESIAN_POINT ( 'NONE',  ( 2.496947748567516889, -4.900535883036019946, 0.8399999999999999689 ) ) ;
#4917 = DIRECTION ( 'NONE',  ( 0.7071067811865467956, 0.7071067811865484609, 0.000000000000000000 ) ) ;
#4918 = CARTESIAN_POINT ( 'NONE',  ( -5.195105386651219348, -2.542276634908102295, 11.74394828327797846 ) ) ;
#4919 = VERTEX_POINT ( 'NONE', #1566 ) ;
#4920 = VECTOR ( 'NONE', #495, 1000.000000000000227 ) ;
#4921 = CARTESIAN_POINT ( 'NONE',  ( 1.500000000000000444, -12.13397459621556607, -1.520833334698926897 ) ) ;
#4922 = EDGE_CURVE ( 'NONE', #6226, #5731, #1024, .T. ) ;
#4923 = APPLICATION_CONTEXT ( 'automotive_design' ) ;
#4924 = AXIS2_PLACEMENT_3D ( 'NONE', #5873, #5824, #8339 ) ;
#4925 =( NAMED_UNIT ( * ) PLANE_ANGLE_UNIT ( ) SI_UNIT ( $, .RADIAN. ) );
#4926 = ORIENTED_EDGE ( 'NONE', *, *, #8093, .T. ) ;
#4927 = VECTOR ( 'NONE', #6324, 1000.000000000000000 ) ;
#4928 = DIRECTION ( 'NONE',  ( -1.000000000000000000, -0.000000000000000000, 0.000000000000000000 ) ) ;
#4929 = AXIS2_PLACEMENT_3D ( 'NONE', #5969, #4098, #2410 ) ;
#4930 = DIRECTION ( 'NONE',  ( 0.000000000000000000, 1.421085471520200372E-14, -1.000000000000000000 ) ) ;
#4931 = PLANE ( 'NONE',  #1351 ) ;
#4932 = PLANE ( 'NONE',  #4724 ) ;
#4933 = CARTESIAN_POINT ( 'NONE',  ( -4.458484982038663169, -0.6162731882459353550, 3.483948283277976898 ) ) ;
#4934 = EDGE_CURVE ( 'NONE', #5853, #9996, #4562, .T. ) ;
#4935 = ORIENTED_EDGE ( 'NONE', *, *, #3101, .T. ) ;
#4936 = EDGE_CURVE ( 'NONE', #1004, #4313, #3201, .T. ) ;
#4937 = CARTESIAN_POINT ( 'NONE',  ( 1.229367062500000385, -12.29022459553277002, -0.3020833340161301339 ) ) ;
#4938 = CARTESIAN_POINT ( 'NONE',  ( 5.432285873273257515, 0.8603895577212793411, 8.679999999999997939 ) ) ;
#4939 = CARTESIAN_POINT ( 'NONE',  ( 3.099999999999998757, 0.000000000000000000, 0.000000000000000000 ) ) ;
#4940 = CARTESIAN_POINT ( 'NONE',  ( 3.889087296526005488, 3.889087296526018811, 8.400000000000000355 ) ) ;
#4941 = DIRECTION ( 'NONE',  ( -1.000000000000000000, -0.000000000000000000, -0.000000000000000000 ) ) ;
#4942 = CYLINDRICAL_SURFACE ( 'NONE', #1453, 1.500000000000000222 ) ;
#4943 = PLANE ( 'NONE',  #365 ) ;
#4944 = VERTEX_POINT ( 'NONE', #2413 ) ;
#4945 = CARTESIAN_POINT ( 'NONE',  ( 3.119207202478379681, 3.244753828200549695, 6.596051716722022285 ) ) ;
#4946 = EDGE_CURVE ( 'NONE', #6306, #8274, #876, .T. ) ;
#4947 = DIRECTION ( 'NONE',  ( 0.000000000000000000, 1.000000000000000000, -1.026972870230479989E-15 ) ) ;
#4948 = CARTESIAN_POINT ( 'NONE',  ( 1.963858260114715870, -4.049832306626327316, 8.243948283277976685 ) ) ;
#4949 = DIRECTION ( 'NONE',  ( 0.000000000000000000, 0.000000000000000000, 1.000000000000000000 ) ) ;
#4950 = VERTEX_POINT ( 'NONE', #10427 ) ;
#4951 = ORIENTED_EDGE ( 'NONE', *, *, #2007, .F. ) ;
#4952 = LINE ( 'NONE', #5106, #10029 ) ;
#4953 = CARTESIAN_POINT ( 'NONE',  ( 10.00000000000000000, -5.233522515400054864, -4.720195129223331065 ) ) ;
#4954 = ORIENTED_EDGE ( 'NONE', *, *, #4014, .T. ) ;
#4955 = ADVANCED_FACE ( 'NONE', ( #4102 ), #9687, .T. ) ;
#4956 = FACE_OUTER_BOUND ( 'NONE', #4747, .T. ) ;
#4957 = PLANE ( 'NONE',  #3218 ) ;
#4958 = ORIENTED_EDGE ( 'NONE', *, *, #10066, .F. ) ;
#4959 = CARTESIAN_POINT ( 'NONE',  ( 0.6162731882459174804, 4.458484982038668498, 9.116051716722020970 ) ) ;
#4960 = PLANE ( 'NONE',  #10228 ) ;
#4961 = ORIENTED_EDGE ( 'NONE', *, *, #4526, .T. ) ;
#4962 = ORIENTED_EDGE ( 'NONE', *, *, #808, .T. ) ;
#4963 = VECTOR ( 'NONE', #1940, 1000.000000000000000 ) ;
#4964 = CARTESIAN_POINT ( 'NONE',  ( 0.4444353696672553311, -7.750000000000000000, 0.000000000000000000 ) ) ;
#4965 = EDGE_CURVE ( 'NONE', #1248, #9930, #6376, .T. ) ;
#4966 = CARTESIAN_POINT ( 'NONE',  ( 0.7500000000000003331, -11.70096189432334732, -0.4166666666666667407 ) ) ;
#4967 = ORIENTED_EDGE ( 'NONE', *, *, #3555, .F. ) ;
#4968 = CARTESIAN_POINT ( 'NONE',  ( 5.432285873273257515, 0.8603895577212793411, 0.2799999999999999156 ) ) ;
#4969 = CARTESIAN_POINT ( 'NONE',  ( 5.711843387010018702, -0.9046671180729751738, 3.219999999999999751 ) ) ;
#4970 = CARTESIAN_POINT ( 'NONE',  ( -4.860232935257354114, 2.576046737280751842, 9.363948283277975904 ) ) ;
#4971 = ORIENTED_EDGE ( 'NONE', *, *, #5102, .F. ) ;
#4972 = CARTESIAN_POINT ( 'NONE',  ( -0.6146835312500006365, -14.06466310670085562, -0.3854166673494634487 ) ) ;
#4973 = VECTOR ( 'NONE', #2762, 1000.000000000000000 ) ;
#4974 = ORIENTED_EDGE ( 'NONE', *, *, #8446, .F. ) ;
#4975 = CARTESIAN_POINT ( 'NONE',  ( 8.000000000000001776, 7.008469740302802897, 0.7425307242148025955 ) ) ;
#4976 = EDGE_CURVE ( 'NONE', #3364, #8683, #5630, .T. ) ;
#4977 = CARTESIAN_POINT ( 'NONE',  ( 4.404961046766194599, 6.000000000000000000, 0.000000000000000000 ) ) ;
#4978 = DIRECTION ( 'NONE',  ( 0.3420201433256627732, 0.9396926207859105373, 0.000000000000000000 ) ) ;
#4979 = VERTEX_POINT ( 'NONE', #78 ) ;
#4980 = AXIS2_PLACEMENT_3D ( 'NONE', #8947, #2327, #9709 ) ;
#4981 = CARTESIAN_POINT ( 'NONE',  ( 5.999999999999999112, -27.00000000000000711, -4.000000000000000000 ) ) ;
#4982 = CARTESIAN_POINT ( 'NONE',  ( -1.229367062500000163, -13.70977540446723708, -2.052083334016129967 ) ) ;
#4983 = CARTESIAN_POINT ( 'NONE',  ( -4.658724279160018078, 0.8323763977770419764, 0.8239482832779764232 ) ) ;
#4984 = ORIENTED_EDGE ( 'NONE', *, *, #3777, .T. ) ;
#4985 = CARTESIAN_POINT ( 'NONE',  ( 30.00000000000001066, -25.00000000000000000, 0.000000000000000000 ) ) ;
#4986 = CARTESIAN_POINT ( 'NONE',  ( -3.889087296526005044, -3.889087296526019255, 1.399999999999999689 ) ) ;
#4987 = PRESENTATION_LAYER_ASSIGNMENT (  '', '', ( #2114 ) ) ;
#4988 = VECTOR ( 'NONE', #5147, 1000.000000000000000 ) ;
#4989 = LINE ( 'NONE', #965, #8877 ) ;
#4990 = CARTESIAN_POINT ( 'NONE',  ( 2.496947748567516889, -4.900535883036019946, 12.03999999999999915 ) ) ;
#4991 = AXIS2_PLACEMENT_3D ( 'NONE', #8377, #8275, #1001 ) ;
#4992 = ADVANCED_FACE ( 'NONE', ( #4000 ), #765, .T. ) ;
#4993 = FACE_OUTER_BOUND ( 'NONE', #5049, .T. ) ;
#4994 = DIRECTION ( 'NONE',  ( 0.000000000000000000, -7.228014483236699822E-18, -1.000000000000000000 ) ) ;
#4995 = DIRECTION ( 'NONE',  ( 1.000000000000000000, 2.312964634635742957E-16, 0.000000000000000000 ) ) ;
#4996 = EDGE_CURVE ( 'NONE', #8513, #897, #6605, .T. ) ;
#4997 = DIRECTION ( 'NONE',  ( -0.000000000000000000, -0.000000000000000000, 1.000000000000000000 ) ) ;
#4998 = CARTESIAN_POINT ( 'NONE',  ( 4.049832306626335310, -1.963858260114701215, 4.356051716722023848 ) ) ;
#4999 = DIRECTION ( 'NONE',  ( 0.000000000000000000, 0.000000000000000000, 1.000000000000000000 ) ) ;
#5000 = CIRCLE ( 'NONE', #2635, 1.599999999999998979 ) ;
#5001 = CARTESIAN_POINT ( 'NONE',  ( -2.231261971483764484, -4.173491630687871101, 8.663948283277974838 ) ) ;
#5002 = CARTESIAN_POINT ( 'NONE',  ( 0.000000000000000000, 0.000000000000000000, 0.000000000000000000 ) ) ;
#5003 = VERTEX_POINT ( 'NONE', #8876 ) ;
#5004 = EDGE_CURVE ( 'NONE', #7675, #4718, #4046, .T. ) ;
#5005 = CARTESIAN_POINT ( 'NONE',  ( 3.826313983664925811, 3.951860609387098044, 6.596051716722022285 ) ) ;
#5006 = EDGE_CURVE ( 'NONE', #6611, #6335, #9361, .T. ) ;
#5007 = CARTESIAN_POINT ( 'NONE',  ( -2.000000000000015099, 35.00000000000000000, 3.999999999999986233 ) ) ;
#5008 = VECTOR ( 'NONE', #1168, 1000.000000000000000 ) ;
#5009 = CARTESIAN_POINT ( 'NONE',  ( 27.00000000000001066, -25.00000000000000000, 1.999999999999997780 ) ) ;
#5010 = ORIENTED_EDGE ( 'NONE', *, *, #6094, .T. ) ;
#5011 = CARTESIAN_POINT ( 'NONE',  ( 11.30300220323380600, -10.00000000000000000, 0.000000000000000000 ) ) ;
#5012 = CARTESIAN_POINT ( 'NONE',  ( 24.68830583033274806, -7.750000000000000000, -12.00000000000000000 ) ) ;
#5013 = ORIENTED_EDGE ( 'NONE', *, *, #5820, .T. ) ;
#5014 = CARTESIAN_POINT ( 'NONE',  ( 3.119207202478379681, 3.244753828200549695, 12.19605171672202282 ) ) ;
#5015 = DIRECTION ( 'NONE',  ( 1.000000000000000000, 0.000000000000000000, -0.000000000000000000 ) ) ;
#5016 = ORIENTED_EDGE ( 'NONE', *, *, #2759, .F. ) ;
#5017 = ADVANCED_FACE ( 'NONE', ( #5350 ), #2975, .F. ) ;
#5018 = SURFACE_STYLE_FILL_AREA ( #7244 ) ;
#5019 = ORIENTED_EDGE ( 'NONE', *, *, #7643, .F. ) ;
#5020 = CARTESIAN_POINT ( 'NONE',  ( 1.999999999999987121, 15.00000000000000355, 4.000000000000008882 ) ) ;
#5021 = CARTESIAN_POINT ( 'NONE',  ( 1.999999999999987121, 15.00000000000000355, 4.000000000000008882 ) ) ;
#5022 = EDGE_LOOP ( 'NONE', ( #1626, #727, #3315, #2657 ) ) ;
#5023 = CARTESIAN_POINT ( 'NONE',  ( -2.542276634908081423, -5.195105386651227342, 2.256051716722022871 ) ) ;
#5024 = CARTESIAN_POINT ( 'NONE',  ( -0.8603895577212598011, -5.432285873273260179, 1.119999999999999885 ) ) ;
#5025 = CARTESIAN_POINT ( 'NONE',  ( -0.8124729078102072011, 5.726445515403652209, 12.58394828327797477 ) ) ;
#5026 = ORIENTED_EDGE ( 'NONE', *, *, #6178, .F. ) ;
#5027 = CARTESIAN_POINT ( 'NONE',  ( 0.6146835312500001924, -11.93533689329915326, -0.6354166673494632267 ) ) ;
#5028 = ORIENTED_EDGE ( 'NONE', *, *, #3949, .F. ) ;
#5029 = DIRECTION ( 'NONE',  ( -0.000000000000000000, -0.000000000000000000, -1.000000000000000000 ) ) ;
#5030 = CARTESIAN_POINT ( 'NONE',  ( 8.000000000000001776, -6.700937042937042065, 0.8165525598867396928 ) ) ;
#5031 = DIRECTION ( 'NONE',  ( 0.3420201433256627732, 0.9396926207859105373, 0.000000000000000000 ) ) ;
#5032 = EDGE_LOOP ( 'NONE', ( #42, #848, #3166, #4379 ) ) ;
#5033 = CARTESIAN_POINT ( 'NONE',  ( 1.300000000000000044, 0.7390083445627193548, -1.280000000000000693 ) ) ;
#5034 = CARTESIAN_POINT ( 'NONE',  ( 1.229367062500000163, -13.70977540446723886, -1.385416667349463449 ) ) ;
#5035 = CARTESIAN_POINT ( 'NONE',  ( 3.969226411068985882, -2.122056237541205981, 2.363948283277975904 ) ) ;
#5036 = ORIENTED_EDGE ( 'NONE', *, *, #5429, .F. ) ;
#5037 = DIRECTION ( 'NONE',  ( -1.000000000000000000, -0.000000000000000000, -0.000000000000000000 ) ) ;
#5038 = CARTESIAN_POINT ( 'NONE',  ( -5.711843387010018702, 0.9046671180729746187, 4.620000000000000107 ) ) ;
#5039 = DIRECTION ( 'NONE',  ( 1.000000000000000000, 0.000000000000000000, -0.000000000000000000 ) ) ;
#5040 = CARTESIAN_POINT ( 'NONE',  ( 5.152728359536493663, 2.625446233515533745, 8.539999999999999147 ) ) ;
#5041 = DIRECTION ( 'NONE',  ( 0.000000000000000000, 0.000000000000000000, -1.000000000000000000 ) ) ;
#5042 = DIRECTION ( 'NONE',  ( 0.000000000000000000, 1.000000000000000000, -7.228014483236699822E-18 ) ) ;
#5043 = LINE ( 'NONE', #7647, #4988 ) ;
#5044 = CARTESIAN_POINT ( 'NONE',  ( 4.173491630687861331, 2.231261971483781359, 3.936051716722023031 ) ) ;
#5045 = DIRECTION ( 'NONE',  ( 0.000000000000000000, 0.4999999999999991673, -0.8660254037844391517 ) ) ;
#5046 = ADVANCED_FACE ( 'NONE', ( #9608 ), #8592, .T. ) ;
#5047 = CARTESIAN_POINT ( 'NONE',  ( 0.6479879772514793856, -4.687928535947285091, 2.783948283277976277 ) ) ;
#5048 = CARTESIAN_POINT ( 'NONE',  ( 0.000000000000000000, -13.00000000000000533, 2.000000000000000000 ) ) ;
#5049 = EDGE_LOOP ( 'NONE', ( #7137, #1513, #8756, #9433 ) ) ;
#5050 = CARTESIAN_POINT ( 'NONE',  ( -4.155232146225753098, 4.023224611898306158, 5.896051716722023883 ) ) ;
#5051 = FACE_OUTER_BOUND ( 'NONE', #5817, .T. ) ;
#5052 = PLANE ( 'NONE',  #8326 ) ;
#5053 = VERTEX_POINT ( 'NONE', #7095 ) ;
#5054 = CARTESIAN_POINT ( 'NONE',  ( 0.7401821875142697849, -4.673326407553650697, 0.9799999999999997602 ) ) ;
#5055 = SURFACE_STYLE_FILL_AREA ( #9145 ) ;
#5056 = VERTEX_POINT ( 'NONE', #10352 ) ;
#5057 = ADVANCED_FACE ( 'NONE', ( #2234 ), #3759, .T. ) ;
#5058 = ADVANCED_FACE ( 'NONE', ( #3077 ), #6989, .F. ) ;
#5059 = AXIS2_PLACEMENT_3D ( 'NONE', #4440, #7072, #6024 ) ;
#5060 = CARTESIAN_POINT ( 'NONE',  ( 4.430710083317573655, 0.7916369971161595354, 12.47605171672202218 ) ) ;
#5061 = CARTESIAN_POINT ( 'NONE',  ( 0.6146835312499993043, -14.06466310670085562, -2.427083334016129967 ) ) ;
#5062 = VERTEX_POINT ( 'NONE', #8748 ) ;
#5063 = ORIENTED_EDGE ( 'NONE', *, *, #8869, .F. ) ;
#5064 = CARTESIAN_POINT ( 'NONE',  ( 8.000000000000001776, 1.418488851014483076, -6.085876303339363247 ) ) ;
#5065 = DIRECTION ( 'NONE',  ( 0.000000000000000000, 1.000000000000000000, -0.000000000000000000 ) ) ;
#5066 = ORIENTED_EDGE ( 'NONE', *, *, #2948, .F. ) ;
#5067 = AXIS2_PLACEMENT_3D ( 'NONE', #9016, #9664, #959 ) ;
#5068 = CARTESIAN_POINT ( 'NONE',  ( 2.625446233515515537, 5.152728359536502545, 11.05999999999999872 ) ) ;
#5069 = CARTESIAN_POINT ( 'NONE',  ( -0.9046671180729963790, 5.711843387010016926, 7.979999999999999538 ) ) ;
#5070 = CARTESIAN_POINT ( 'NONE',  ( 2.496947748567516889, -4.900535883036019946, 12.03999999999999915 ) ) ;
#5071 = ORIENTED_EDGE ( 'NONE', *, *, #5201, .F. ) ;
#5072 = EDGE_CURVE ( 'NONE', #1747, #9420, #7149, .T. ) ;
#5073 = CARTESIAN_POINT ( 'NONE',  ( -1.229367062500000385, -13.70977540446723886, -1.427083334016129745 ) ) ;
#5074 = AXIS2_PLACEMENT_3D ( 'NONE', #159, #9221, #5816 ) ;
#5075 = SURFACE_STYLE_USAGE ( .BOTH. , #5286 ) ;
#5076 =( GEOMETRIC_REPRESENTATION_CONTEXT ( 3 ) GLOBAL_UNCERTAINTY_ASSIGNED_CONTEXT ( ( #6065 ) ) GLOBAL_UNIT_ASSIGNED_CONTEXT ( ( #2782, #2732, #299 ) ) REPRESENTATION_CONTEXT ( 'NONE', 'WORKASPACE' ) );
#5077 = ORIENTED_EDGE ( 'NONE', *, *, #9315, .F. ) ;
#5078 = CARTESIAN_POINT ( 'NONE',  ( -5.999999999999999112, 26.99999999999999289, -17.00000000000000000 ) ) ;
#5079 = LINE ( 'NONE', #5917, #5403 ) ;
#5080 = ORIENTED_EDGE ( 'NONE', *, *, #1379, .T. ) ;
#5081 = LINE ( 'NONE', #270, #6922 ) ;
#5082 = VECTOR ( 'NONE', #2789, 1000.000000000000000 ) ;
#5083 = CARTESIAN_POINT ( 'NONE',  ( 1.229367062500000163, -12.29022459553277002, -0.8020833340161301894 ) ) ;
#5084 = CARTESIAN_POINT ( 'NONE',  ( 0.7401821875142697849, -4.673326407553650697, 12.17999999999999439 ) ) ;
#5085 = ORIENTED_EDGE ( 'NONE', *, *, #1646, .T. ) ;
#5086 = VECTOR ( 'NONE', #1452, 1000.000000000000000 ) ;
#5087 = CARTESIAN_POINT ( 'NONE',  ( 21.54671318033274829, -7.750000000000000000, -12.00000000000000000 ) ) ;
#5088 = CARTESIAN_POINT ( 'NONE',  ( -5.711843387010018702, 0.9046671180729746187, 10.21999999999999709 ) ) ;
#5089 = VECTOR ( 'NONE', #903, 1000.000000000000000 ) ;
#5090 = CARTESIAN_POINT ( 'NONE',  ( 15.00000000000000000, 19.99999999999999645, -5.999999999999999112 ) ) ;
#5091 = AXIS2_PLACEMENT_3D ( 'NONE', #1448, #6260, #5574 ) ;
#5092 = CARTESIAN_POINT ( 'NONE',  ( 4.089228379062037178, -4.089228379062022967, 6.299999999999998934 ) ) ;
#5093 = AXIS2_PLACEMENT_3D ( 'NONE', #464, #4532, #6014 ) ;
#5094 = CARTESIAN_POINT ( 'NONE',  ( 7.555798540716556211, 6.025400000000000311, -12.00000000000000000 ) ) ;
#5095 = CARTESIAN_POINT ( 'NONE',  ( 0.000000000000000000, -10.00000000000000000, -12.00000000000000000 ) ) ;
#5096 = AXIS2_PLACEMENT_3D ( 'NONE', #1184, #5206, #4412 ) ;
#5097 = CARTESIAN_POINT ( 'NONE',  ( -2.000000000000000000, 0.000000000000000000, 0.000000000000000000 ) ) ;
#5098 = CARTESIAN_POINT ( 'NONE',  ( -4.173491630687863108, -2.231261971483782691, 5.336051716722022498 ) ) ;
#5099 = DIRECTION ( 'NONE',  ( -0.000000000000000000, -0.000000000000000000, 1.000000000000000000 ) ) ;
#5100 = SHAPE_REPRESENTATION ( 'BR-002', ( #4310, #9066, #1274, #8388, #9919, #10088, #3639, #4145, #9406, #5493, #936, #7708, #7020 ), #8895 ) ;
#5101 = CARTESIAN_POINT ( 'NONE',  ( -0.6479879772514802738, 4.687928535947285091, 1.383948283277976365 ) ) ;
#5102 = EDGE_CURVE ( 'NONE', #1286, #4614, #6357, .T. ) ;
#5103 = CARTESIAN_POINT ( 'NONE',  ( 0.6146835312499993043, -14.06466310670085562, -2.302083334016129967 ) ) ;
#5104 = ORIENTED_EDGE ( 'NONE', *, *, #10254, .T. ) ;
#5105 = CARTESIAN_POINT ( 'NONE',  ( 2.576046737280769605, -4.860232935257343456, 1.836051716722023386 ) ) ;
#5106 = CARTESIAN_POINT ( 'NONE',  ( 30.00000000000001066, 35.00000000000001421, 9.000000000000000000 ) ) ;
#5107 = EDGE_CURVE ( 'NONE', #3824, #9213, #7799, .T. ) ;
#5108 = CYLINDRICAL_SURFACE ( 'NONE', #1545, 8.500000000000000000 ) ;
#5109 = VERTEX_POINT ( 'NONE', #2335 ) ;
#5110 = CARTESIAN_POINT ( 'NONE',  ( 0.000000000000000000, -10.00000000000000000, -12.00000000000000000 ) ) ;
#5111 = CARTESIAN_POINT ( 'NONE',  ( 25.00000000000000000, 0.000000000000000000, 0.000000000000000000 ) ) ;
#5112 = CARTESIAN_POINT ( 'NONE',  ( -4.049832306626335310, 1.963858260114700327, 5.756051716722022427 ) ) ;
#5113 = CARTESIAN_POINT ( 'NONE',  ( 23.86937280323380506, -10.00000000000000178, -12.00000000000000000 ) ) ;
#5114 = ORIENTED_EDGE ( 'NONE', *, *, #6371, .F. ) ;
#5115 = DIRECTION ( 'NONE',  ( 6.123233995736766036E-17, 0.000000000000000000, -1.000000000000000000 ) ) ;
#5116 = VERTEX_POINT ( 'NONE', #5558 ) ;
#5117 = EDGE_CURVE ( 'NONE', #5532, #8167, #686, .T. ) ;
#5118 = DIRECTION ( 'NONE',  ( -0.000000000000000000, -1.000000000000000000, -0.000000000000000000 ) ) ;
#5119 = ORIENTED_EDGE ( 'NONE', *, *, #10139, .F. ) ;
#5120 = CARTESIAN_POINT ( 'NONE',  ( 5.110351332421769754, 2.708615832122969191, 3.936051716722023031 ) ) ;
#5121 = CARTESIAN_POINT ( 'NONE',  ( 5.711843387010018702, -0.9046671180729751738, 6.019999999999999574 ) ) ;
#5122 = CARTESIAN_POINT ( 'NONE',  ( 4.089228379062037178, -4.089228379062022967, 6.299999999999999822 ) ) ;
#5123 = VERTEX_POINT ( 'NONE', #6938 ) ;
#5124 = CARTESIAN_POINT ( 'NONE',  ( 0.6146835312500001924, -11.93533689329915326, -2.135416667349463449 ) ) ;
#5125 = AXIS2_PLACEMENT_3D ( 'NONE', #6203, #8811, #5621 ) ;
#5126 = FILL_AREA_STYLE ('',( #214 ) ) ;
#5127 = ORIENTED_EDGE ( 'NONE', *, *, #2607, .F. ) ;
#5128 = ADVANCED_FACE ( 'NONE', ( #5507 ), #1381, .F. ) ;
#5129 = CYLINDRICAL_SURFACE ( 'NONE', #4991, 3.000000000000000000 ) ;
#5130 = EDGE_CURVE ( 'NONE', #5902, #8074, #7748, .T. ) ;
#5131 = CARTESIAN_POINT ( 'NONE',  ( 1.999999999999980904, 35.00000000000000000, -6.000000000000000000 ) ) ;
#5132 = ORIENTED_EDGE ( 'NONE', *, *, #457, .T. ) ;
#5133 = DIRECTION ( 'NONE',  ( -0.7043149233066458015, 0.7043149233066440251, -0.08877487040322762368 ) ) ;
#5134 = DIRECTION ( 'NONE',  ( 0.3420201433256627732, -0.9396926207859105373, 0.000000000000000000 ) ) ;
#5135 = VECTOR ( 'NONE', #9025, 1000.000000000000000 ) ;
#5136 = CARTESIAN_POINT ( 'NONE',  ( 1.229367062500000163, -13.70977540446723886, -0.3854166673494634487 ) ) ;
#5137 = CARTESIAN_POINT ( 'NONE',  ( 4.658724279160018966, -0.8323763977770426425, 7.823948283277974980 ) ) ;
#5138 = VERTEX_POINT ( 'NONE', #10195 ) ;
#5139 = FACE_OUTER_BOUND ( 'NONE', #9744, .T. ) ;
#5140 = CARTESIAN_POINT ( 'NONE',  ( 5.711843387010018702, -0.9046671180729751738, 11.61999999999999922 ) ) ;
#5141 = CARTESIAN_POINT ( 'NONE',  ( 10.00000000000000178, 0.000000000000000000, 2.000000000000000000 ) ) ;
#5142 = COLOUR_RGB ( '', 0.31764706, 0.68627451, 0.89019608) ;
#5143 = EDGE_CURVE ( 'NONE', #4307, #1402, #2922, .T. ) ;
#5144 = CARTESIAN_POINT ( 'NONE',  ( -5.432285873273256627, -0.8603895577212797852, 7.279999999999999361 ) ) ;
#5145 = DIRECTION ( 'NONE',  ( 0.3420201433256627732, 0.9396926207859105373, 0.000000000000000000 ) ) ;
#5146 = DIRECTION ( 'NONE',  ( 0.000000000000000000, -1.000000000000000000, 0.000000000000000000 ) ) ;
#5147 = DIRECTION ( 'NONE',  ( 0.000000000000000000, 0.000000000000000000, 1.000000000000000000 ) ) ;
#5148 = CARTESIAN_POINT ( 'NONE',  ( -4.673326407553653361, 0.7401821875142517992, 1.819999999999999396 ) ) ;
#5149 = CARTESIAN_POINT ( 'NONE',  ( 1.229367062499999719, -13.70977540446724063, -1.260416667349463449 ) ) ;
#5150 = CARTESIAN_POINT ( 'NONE',  ( -0.9480714621563718358, -5.418398423912716311, 2.923948283277976401 ) ) ;
#5151 = CARTESIAN_POINT ( 'NONE',  ( -2.607672531582950546E-16, -14.41955080893447416, -1.843750000682796708 ) ) ;
#5152 = VECTOR ( 'NONE', #2445, 1000.000000000000000 ) ;
#5153 = EDGE_LOOP ( 'NONE', ( #10216, #10447 ) ) ;
#5154 = CARTESIAN_POINT ( 'NONE',  ( 0.9968613283357860011, -5.697241258616382531, 1.976051716722022844 ) ) ;
#5155 = ORIENTED_EDGE ( 'NONE', *, *, #468, .T. ) ;
#5156 = LINE ( 'NONE', #2726, #777 ) ;
#5157 = CARTESIAN_POINT ( 'NONE',  ( 1.300000000000000044, -0.7390083445627200209, 1.280000000000001137 ) ) ;
#5158 = ADVANCED_FACE ( 'NONE', ( #3813 ), #583, .T. ) ;
#5159 = ORIENTED_EDGE ( 'NONE', *, *, #447, .T. ) ;
#5160 = CONICAL_SURFACE ( 'NONE', #7371, 1.219500000000000028, 0.7853981633974680410 ) ;
#5161 = CARTESIAN_POINT ( 'NONE',  ( -4.444597532678119300, -0.7039550926810477227, 10.07999999999999829 ) ) ;
#5162 = DIRECTION ( 'NONE',  ( 0.000000000000000000, 0.000000000000000000, -1.000000000000000000 ) ) ;
#5163 = CARTESIAN_POINT ( 'NONE',  ( -2.064922774268895811, -4.258245684917318918, 13.45605171672202260 ) ) ;
#5164 = CARTESIAN_POINT ( 'NONE',  ( -1.500000000000002220, -13.86602540378444282, -1.270833334698927120 ) ) ;
#5165 = ORIENTED_EDGE ( 'NONE', *, *, #6723, .F. ) ;
#5166 = DIRECTION ( 'NONE',  ( 0.000000000000000000, -7.847870334214135379E-05, -0.9999999969205466410 ) ) ;
#5167 = ORIENTED_EDGE ( 'NONE', *, *, #338, .T. ) ;
#5168 = LINE ( 'NONE', #1144, #2126 ) ;
#5169 = VECTOR ( 'NONE', #2247, 1000.000000000000000 ) ;
#5170 = CYLINDRICAL_SURFACE ( 'NONE', #8812, 2.500000000000000000 ) ;
#5171 = ORIENTED_EDGE ( 'NONE', *, *, #8874, .F. ) ;
#5172 = CARTESIAN_POINT ( 'NONE',  ( -0.8603895577212598011, -5.432285873273260179, 12.31999999999999851 ) ) ;
#5173 = CARTESIAN_POINT ( 'NONE',  ( 0.8603895577212593571, 5.432285873273261068, 2.519999999999999574 ) ) ;
#5174 = CARTESIAN_POINT ( 'NONE',  ( -4.900535883036028828, 2.496947748567499126, 10.35999999999999943 ) ) ;
#5175 = EDGE_LOOP ( 'NONE', ( #4058, #3790, #8150, #7322 ) ) ;
#5176 = CIRCLE ( 'NONE', #608, 2.500000000000000000 ) ;
#5177 = CARTESIAN_POINT ( 'NONE',  ( 1.229367062500000385, -12.29022459553277002, -1.177083334016129967 ) ) ;
#5178 = VECTOR ( 'NONE', #7370, 1000.000000000000000 ) ;
#5179 = EDGE_CURVE ( 'NONE', #7785, #4320, #7970, .T. ) ;
#5180 =( LENGTH_UNIT ( ) NAMED_UNIT ( * ) SI_UNIT ( .MILLI., .METRE. ) );
#5181 = VERTEX_POINT ( 'NONE', #9458 ) ;
#5182 = CARTESIAN_POINT ( 'NONE',  ( 8.000000000000001776, -6.200809695932781196, 0.7745709230444935978 ) ) ;
#5183 = CARTESIAN_POINT ( 'NONE',  ( 0.000000000000000000, 18.99999999999999289, 1.249999999999997558 ) ) ;
#5184 = EDGE_LOOP ( 'NONE', ( #3655, #5953, #2268, #10023, #84 ) ) ;
#5185 = CARTESIAN_POINT ( 'NONE',  ( -29.99999999999998934, -13.00000000000000533, 0.000000000000000000 ) ) ;
#5186 = CARTESIAN_POINT ( 'NONE',  ( 4.000000000000000888, 4.438567988583180579, -7.249076783337634389 ) ) ;
#5187 = CARTESIAN_POINT ( 'NONE',  ( -1.229367062500000163, -13.70977540446723708, -0.05208333401612994656 ) ) ;
#5188 = CARTESIAN_POINT ( 'NONE',  ( 5.446173322633801384, 0.7727076532861675284, -0.7160517167220232793 ) ) ;
#5189 = ORIENTED_EDGE ( 'NONE', *, *, #1022, .F. ) ;
#5190 = CARTESIAN_POINT ( 'NONE',  ( -9.000000000000000000, 19.99999999999999645, 17.00000000000000000 ) ) ;
#5191 = EDGE_CURVE ( 'NONE', #7286, #6012, #10206, .T. ) ;
#5192 = EDGE_CURVE ( 'NONE', #3788, #3797, #4563, .T. ) ;
#5193 = CARTESIAN_POINT ( 'NONE',  ( 9.000000000000000000, 19.99999999999999645, 17.00000000000000000 ) ) ;
#5194 = DIRECTION ( 'NONE',  ( -1.000000000000000000, -0.000000000000000000, -0.000000000000000000 ) ) ;
#5195 = CARTESIAN_POINT ( 'NONE',  ( 1.060575238724907038E-16, -11.26794919243112680, -2.875000000000000000 ) ) ;
#5196 = FACE_OUTER_BOUND ( 'NONE', #3496, .T. ) ;
#5197 = CARTESIAN_POINT ( 'NONE',  ( 3.099999999999998757, 0.000000000000000000, -1.600000000000000311 ) ) ;
#5198 = LINE ( 'NONE', #1074, #6589 ) ;
#5199 = CARTESIAN_POINT ( 'NONE',  ( -2.122056237541221968, 3.969226411068977889, 8.836051716722023386 ) ) ;
#5200 = CARTESIAN_POINT ( 'NONE',  ( -1.229367062500000163, -12.29022459553277002, -2.510416667349463449 ) ) ;
#5201 = EDGE_CURVE ( 'NONE', #3542, #1643, #7757, .T. ) ;
#5202 = CARTESIAN_POINT ( 'NONE',  ( 5.697241258616385196, -0.9968613283357656840, 2.223948283277975779 ) ) ;
#5203 = CARTESIAN_POINT ( 'NONE',  ( 0.6146835312499993043, -14.06466310670085562, -1.302083334016129967 ) ) ;
#5204 = ORIENTED_EDGE ( 'NONE', *, *, #4410, .F. ) ;
#5205 = CARTESIAN_POINT ( 'NONE',  ( -4.940838830814703542, 2.417848759854245078, 2.956051716722023492 ) ) ;
#5206 = DIRECTION ( 'NONE',  ( -1.000000000000000000, -0.000000000000000000, -0.000000000000000000 ) ) ;
#5207 = DIRECTION ( 'NONE',  ( 0.000000000000000000, 0.000000000000000000, -1.000000000000000000 ) ) ;
#5208 = VERTEX_POINT ( 'NONE', #4617 ) ;
#5209 = CARTESIAN_POINT ( 'NONE',  ( -3.345732310141667831, 3.345732310141653620, 10.50000000000000000 ) ) ;
#5210 = CARTESIAN_POINT ( 'NONE',  ( 7.206705994753384914, 8.623026469197982991, 0.000000000000000000 ) ) ;
#5211 = CARTESIAN_POINT ( 'NONE',  ( 4.215868657802586128, 2.148092372876346801, 5.739999999999997549 ) ) ;
#5212 = CARTESIAN_POINT ( 'NONE',  ( 0.6146835312499993043, -14.06466310670085562, -0.4270833340161298564 ) ) ;
#5213 = ORIENTED_EDGE ( 'NONE', *, *, #595, .F. ) ;
#5214 = PRODUCT_DEFINITION ( 'UNKNOWN', '', #6846, #2903 ) ;
#5215 = DIRECTION ( 'NONE',  ( 6.123233995736766036E-17, 0.000000000000000000, 1.000000000000000000 ) ) ;
#5216 = ORIENTED_EDGE ( 'NONE', *, *, #3704, .F. ) ;
#5217 = DIRECTION ( 'NONE',  ( 0.000000000000000000, 0.000000000000000000, -1.000000000000000000 ) ) ;
#5218 = PLANE ( 'NONE',  #9856 ) ;
#5219 = DIRECTION ( 'NONE',  ( -1.000000000000000000, -0.000000000000000000, -0.000000000000000000 ) ) ;
#5220 = ORIENTED_EDGE ( 'NONE', *, *, #1982, .T. ) ;
#5221 = CARTESIAN_POINT ( 'NONE',  ( 4.900535883036028828, -2.496947748567499126, 11.75999999999999979 ) ) ;
#5222 = EDGE_CURVE ( 'NONE', #5062, #4078, #5754, .T. ) ;
#5223 = CONICAL_SURFACE ( 'NONE', #999, 1.249999999999997558, 1.029744258676650981 ) ;
#5224 = CARTESIAN_POINT ( 'NONE',  ( -2.625446233515515981, -5.152728359536500768, 9.659999999999994813 ) ) ;
#5225 = CARTESIAN_POINT ( 'NONE',  ( 5.711843387010018702, -0.9046671180729751738, 6.019999999999999574 ) ) ;
#5226 = ORIENTED_EDGE ( 'NONE', *, *, #541, .T. ) ;
#5227 = DIRECTION ( 'NONE',  ( 0.000000000000000000, -0.000000000000000000, 1.000000000000000000 ) ) ;
#5228 = PRODUCT_DEFINITION_CONTEXT ( 'detailed design', #8714, 'design' ) ;
#5229 = EDGE_CURVE ( 'NONE', #2398, #1402, #5264, .T. ) ;
#5230 = FILL_AREA_STYLE_COLOUR ( '', #8549 ) ;
#5231 = AXIS2_PLACEMENT_3D ( 'NONE', #778, #8886, #6593 ) ;
#5232 = ORIENTED_EDGE ( 'NONE', *, *, #2305, .T. ) ;
#5233 = LINE ( 'NONE', #9379, #265 ) ;
#5234 = AXIS2_PLACEMENT_3D ( 'NONE', #9119, #10132, #2067 ) ;
#5235 = CARTESIAN_POINT ( 'NONE',  ( 1.300000000000000044, 0.000000000000000000, 0.000000000000000000 ) ) ;
#5236 = ORIENTED_EDGE ( 'NONE', *, *, #721, .F. ) ;
#5237 = CARTESIAN_POINT ( 'NONE',  ( -2.000000000000000000, -4.147285340411748678, -5.698247474649444477 ) ) ;
#5238 = EDGE_CURVE ( 'NONE', #10028, #2670, #7814, .T. ) ;
#5239 = LINE ( 'NONE', #7787, #9907 ) ;
#5240 = CYLINDRICAL_SURFACE ( 'NONE', #1510, 1.500000000000000222 ) ;
#5241 = CARTESIAN_POINT ( 'NONE',  ( 3.969226411068985882, -2.122056237541205981, 7.963948283277976437 ) ) ;
#5242 = ORIENTED_EDGE ( 'NONE', *, *, #3400, .F. ) ;
#5243 = AXIS2_PLACEMENT_3D ( 'NONE', #2336, #635, #2497 ) ;
#5244 = CYLINDRICAL_SURFACE ( 'NONE', #6777, 1.599999999999998979 ) ;
#5245 = MECHANICAL_DESIGN_GEOMETRIC_PRESENTATION_REPRESENTATION (  '', ( #8470 ), #5751 ) ;
#5246 = DIRECTION ( 'NONE',  ( 0.000000000000000000, 0.000000000000000000, 1.000000000000000000 ) ) ;
#5247 = DIRECTION ( 'NONE',  ( 0.000000000000000000, 0.000000000000000000, 1.000000000000000000 ) ) ;
#5248 = CARTESIAN_POINT ( 'NONE',  ( 10.00000000000000178, 0.000000000000000000, 0.000000000000000000 ) ) ;
#5249 = AXIS2_PLACEMENT_3D ( 'NONE', #408, #5219, #7771 ) ;
#5250 = CARTESIAN_POINT ( 'NONE',  ( 9.869213319667256457, 3.750000000000000000, -12.00000000000000000 ) ) ;
#5251 = EDGE_CURVE ( 'NONE', #8930, #10490, #3721, .T. ) ;
#5252 = VECTOR ( 'NONE', #3942, 1000.000000000000000 ) ;
#5253 = FACE_OUTER_BOUND ( 'NONE', #1967, .T. ) ;
#5254 = EDGE_CURVE ( 'NONE', #244, #6381, #2141, .T. ) ;
#5255 = CARTESIAN_POINT ( 'NONE',  ( 1.300000000000000044, -1.478016689125442706, 1.843143693225357538E-15 ) ) ;
#5256 = CARTESIAN_POINT ( 'NONE',  ( -2.064922774268895811, -4.258245684917318918, 13.45605171672202260 ) ) ;
#5257 = CARTESIAN_POINT ( 'NONE',  ( -0.6146835312500006365, -14.06466310670085562, -2.385416667349463005 ) ) ;
#5258 = VECTOR ( 'NONE', #5637, 1000.000000000000000 ) ;
#5259 = VECTOR ( 'NONE', #1884, 1000.000000000000000 ) ;
#5260 = CARTESIAN_POINT ( 'NONE',  ( -4.658724279160018078, 0.8323763977770419764, 12.02394828327797427 ) ) ;
#5261 = CARTESIAN_POINT ( 'NONE',  ( 0.6146835312499993043, -14.06466310670085562, -0.3020833340161297453 ) ) ;
#5263 = ORIENTED_EDGE ( 'NONE', *, *, #5954, .F. ) ;
#5262 = VECTOR ( 'NONE', #2555, 1000.000000000000000 ) ;
#5264 = LINE ( 'NONE', #8555, #7461 ) ;
#5265 = AXIS2_PLACEMENT_3D ( 'NONE', #1299, #7770, #502 ) ;
#5266 = ADVANCED_FACE ( 'NONE', ( #392 ), #1392, .T. ) ;
#5267 = DIRECTION ( 'NONE',  ( 0.000000000000000000, 1.000000000000000000, 0.000000000000000000 ) ) ;
#5268 = DIRECTION ( 'NONE',  ( 0.000000000000000000, 0.000000000000000000, -1.000000000000000000 ) ) ;
#5269 = DIRECTION ( 'NONE',  ( -1.000000000000000000, -0.000000000000000000, -0.000000000000000000 ) ) ;
#5270 = EDGE_LOOP ( 'NONE', ( #4324, #7506, #8058, #5535, #6570 ) ) ;
#5271 = CARTESIAN_POINT ( 'NONE',  ( 2.042957248827968808, -4.009529358847652603, 9.240000000000000213 ) ) ;
#5272 = CARTESIAN_POINT ( 'NONE',  ( 4.673326407553653361, -0.7401821875142523544, 3.219999999999999751 ) ) ;
#5273 = CARTESIAN_POINT ( 'NONE',  ( -1.229367062500000163, -13.00000000000000533, -1.593750000682796708 ) ) ;
#5274 = ORIENTED_EDGE ( 'NONE', *, *, #1169, .T. ) ;
#5275 = ORIENTED_EDGE ( 'NONE', *, *, #9516, .T. ) ;
#5276 = ADVANCED_FACE ( 'NONE', ( #2827 ), #2188, .F. ) ;
#5277 = LINE ( 'NONE', #4423, #8068 ) ;
#5278 = LINE ( 'NONE', #9309, #9327 ) ;
#5279 = CARTESIAN_POINT ( 'NONE',  ( 10.00000000000000000, 2.429606751577122026, -5.757344182232885466 ) ) ;
#5280 = EDGE_LOOP ( 'NONE', ( #352, #2623, #5290, #950 ) ) ;
#5281 = CARTESIAN_POINT ( 'NONE',  ( 0.9968613283357860011, -5.697241258616382531, 7.576051716722023599 ) ) ;
#5282 = CARTESIAN_POINT ( 'NONE',  ( -5.432285873273256627, -0.8603895577212797852, 10.07999999999999829 ) ) ;
#5283 = CARTESIAN_POINT ( 'NONE',  ( 2.625446233515515537, 5.152728359536502545, 5.459999999999997300 ) ) ;
#5284 = EDGE_LOOP ( 'NONE', ( #3470, #891, #9547, #6343 ) ) ;
#5285 = DIRECTION ( 'NONE',  ( 0.3420201433256627732, -0.9396926207859105373, 0.000000000000000000 ) ) ;
#5286 = SURFACE_SIDE_STYLE ('',( #6818 ) ) ;
#5287 = ORIENTED_EDGE ( 'NONE', *, *, #2662, .F. ) ;
#5288 = CARTESIAN_POINT ( 'NONE',  ( 0.000000000000000000, -19.00000000000000711, -1.249999999999997558 ) ) ;
#5289 = PLANE ( 'NONE',  #1696 ) ;
#5290 = ORIENTED_EDGE ( 'NONE', *, *, #9802, .T. ) ;
#5291 = FACE_OUTER_BOUND ( 'NONE', #8376, .T. ) ;
#5292 = FACE_OUTER_BOUND ( 'NONE', #6595, .T. ) ;
#5293 = CARTESIAN_POINT ( 'NONE',  ( 1.229367062500000163, -13.00000000000000533, 0.1562499993172034307 ) ) ;
#5294 = CARTESIAN_POINT ( 'NONE',  ( 4.258245684917310037, 2.064922774268912686, 7.543948283277975619 ) ) ;
#5295 = VERTEX_POINT ( 'NONE', #5412 ) ;
#5296 = CARTESIAN_POINT ( 'NONE',  ( -2.000000000000000000, 6.226349476952025341, -0.5315761383463619705 ) ) ;
#5297 = VECTOR ( 'NONE', #895, 1000.000000000000000 ) ;
#5298 = DIRECTION ( 'NONE',  ( -1.000000000000000000, -0.000000000000000000, -0.000000000000000000 ) ) ;
#5299 = CARTESIAN_POINT ( 'NONE',  ( 15.26352788033274699, -7.750000000000000000, -12.00000000000000000 ) ) ;
#5300 = EDGE_CURVE ( 'NONE', #7393, #2426, #8316, .T. ) ;
#5301 = CARTESIAN_POINT ( 'NONE',  ( 16.15239861966725599, 3.750000000000000000, -12.00000000000000000 ) ) ;
#5302 = AXIS2_PLACEMENT_3D ( 'NONE', #9604, #1375, #2331 ) ;
#5303 = FACE_OUTER_BOUND ( 'NONE', #1413, .T. ) ;
#5304 = DIRECTION ( 'NONE',  ( 0.000000000000000000, -1.000000000000000000, 0.000000000000000000 ) ) ;
#5305 = DIRECTION ( 'NONE',  ( 0.000000000000000000, 0.000000000000000000, 1.000000000000000000 ) ) ;
#5306 = CARTESIAN_POINT ( 'NONE',  ( 2.042957248827968808, -4.009529358847652603, 0.8399999999999999689 ) ) ;
#5307 = CARTESIAN_POINT ( 'NONE',  ( 1.229367062499999719, -13.70977540446724063, -0.2604166673494632822 ) ) ;
#5308 = CARTESIAN_POINT ( 'NONE',  ( -4.258245684917310925, -2.064922774268914019, 11.74394828327797846 ) ) ;
#5309 = CIRCLE ( 'NONE', #9044, 1.249999999999987121 ) ;
#5310 = CARTESIAN_POINT ( 'NONE',  ( -1.229367062500000163, -13.70977540446723708, 0.07291666598387017140 ) ) ;
#5311 = EDGE_CURVE ( 'NONE', #8939, #3364, #17, .T. ) ;
#5312 = ORIENTED_EDGE ( 'NONE', *, *, #5772, .F. ) ;
#5313 = DIRECTION ( 'NONE',  ( 1.000000000000000000, -0.000000000000000000, -0.000000000000000000 ) ) ;
#5314 = LINE ( 'NONE', #4513, #8490 ) ;
#5315 = LINE ( 'NONE', #4356, #9593 ) ;
#5316 = CARTESIAN_POINT ( 'NONE',  ( 0.000000000000000000, 6.000000000000000000, -12.00000000000000000 ) ) ;
#5317 = ORIENTED_EDGE ( 'NONE', *, *, #1708, .T. ) ;
#5318 = CARTESIAN_POINT ( 'NONE',  ( 16.97133164676619899, 6.000000000000000888, 0.000000000000000000 ) ) ;
#5319 = CARTESIAN_POINT ( 'NONE',  ( -3.181980515339458027, -3.181980515339470905, 1.399999999999999689 ) ) ;
#5320 = EDGE_CURVE ( 'NONE', #1744, #5526, #594, .T. ) ;
#5321 = CARTESIAN_POINT ( 'NONE',  ( 0.6146835312499993043, -14.06466310670085562, -1.927083334016129967 ) ) ;
#5322 = EDGE_CURVE ( 'NONE', #10163, #8333, #9294, .T. ) ;
#5323 =( GEOMETRIC_REPRESENTATION_CONTEXT ( 3 ) GLOBAL_UNCERTAINTY_ASSIGNED_CONTEXT ( ( #9267 ) ) GLOBAL_UNIT_ASSIGNED_CONTEXT ( ( #5180, #7681, #8427 ) ) REPRESENTATION_CONTEXT ( 'NONE', 'WORKASPACE' ) );
#5324 = ORIENTED_EDGE ( 'NONE', *, *, #8576, .F. ) ;
#5325 = ORIENTED_EDGE ( 'NONE', *, *, #4277, .F. ) ;
#5326 = LINE ( 'NONE', #8612, #701 ) ;
#5327 = VECTOR ( 'NONE', #7914, 1000.000000000000000 ) ;
#5328 = DIRECTION ( 'NONE',  ( 1.156482317317871478E-16, -1.000000000000000000, -0.000000000000000000 ) ) ;
#5329 = ORIENTED_EDGE ( 'NONE', *, *, #10232, .F. ) ;
#5330 = CARTESIAN_POINT ( 'NONE',  ( 2.542276634908080535, 5.195105386651229118, 12.05605171672202047 ) ) ;
#5331 = DIRECTION ( 'NONE',  ( 0.000000000000000000, 1.000000000000000000, 0.000000000000000000 ) ) ;
#5332 = VERTEX_POINT ( 'NONE', #4460 ) ;
#5333 = PLANE ( 'NONE',  #9169 ) ;
#5334 = EDGE_CURVE ( 'NONE', #520, #5208, #6953, .T. ) ;
#5335 = AXIS2_PLACEMENT_3D ( 'NONE', #7029, #1472, #8000 ) ;
#5336 = ORIENTED_EDGE ( 'NONE', *, *, #9217, .T. ) ;
#5337 = EDGE_LOOP ( 'NONE', ( #9317, #9793, #44, #3686 ) ) ;
#5338 = DIRECTION ( 'NONE',  ( 1.000000000000000000, 0.000000000000000000, -0.000000000000000000 ) ) ;
#5339 = FACE_OUTER_BOUND ( 'NONE', #6445, .T. ) ;
#5340 = ORIENTED_EDGE ( 'NONE', *, *, #4036, .T. ) ;
#5341 = CYLINDRICAL_SURFACE ( 'NONE', #838, 6.248999999999999666 ) ;
#5342 = CIRCLE ( 'NONE', #3820, 3.000000000000000000 ) ;
#5343 = DIRECTION ( 'NONE',  ( 0.000000000000000000, 0.000000000000000000, 1.000000000000000000 ) ) ;
#5344 = CARTESIAN_POINT ( 'NONE',  ( -4.860232935257354114, 2.576046737280751842, 6.563948283277975193 ) ) ;
#5345 = ORIENTED_EDGE ( 'NONE', *, *, #83, .F. ) ;
#5346 = CARTESIAN_POINT ( 'NONE',  ( 11.30300220323380600, 6.000000000000000000, 0.000000000000000000 ) ) ;
#5347 = CARTESIAN_POINT ( 'NONE',  ( 6.727620669667255804, -7.750000000000000000, -12.00000000000000000 ) ) ;
#5348 = CARTESIAN_POINT ( 'NONE',  ( 1.229367062500000163, -13.00000000000000533, -2.843750000682796486 ) ) ;
#5349 = CARTESIAN_POINT ( 'NONE',  ( 0.7500000000000003331, -11.70096189432334732, -2.916666666666666963 ) ) ;
#5350 = FACE_OUTER_BOUND ( 'NONE', #9570, .T. ) ;
#5351 = DIRECTION ( 'NONE',  ( -0.000000000000000000, -0.000000000000000000, 1.000000000000000000 ) ) ;
#5352 = DIRECTION ( 'NONE',  ( 0.000000000000000000, -0.000000000000000000, 1.000000000000000000 ) ) ;
#5353 = LINE ( 'NONE', #2132, #9617 ) ;
#5354 = CARTESIAN_POINT ( 'NONE',  ( 3.119207202478379681, 3.244753828200549695, 14.99605171672202175 ) ) ;
#5355 =( BOUNDED_CURVE ( )  B_SPLINE_CURVE ( 2, ( #8151, #6438, #7450, #193, #91, #4111, #4903, #5054, #9698, #2424, #3266, #9851, #3421, #4851, #3317, #5641, #4011, #1731, #7239, #8096, #6644, #6543, #9794, #933, #825, #4056, #7293, #40, #6489, #2522, #9746, #5741, #2577, #2476, #5792, #9046, #5690, #1675, #3365, #8991, #7397, #139, #4360, #3472, #4309, #7601, #348, #6046, #5945, #298, #1137, #9253, #1086, #2041, #6698, #1989, #2093, #8509, #3574, #9952, #7556, #2832, #6799, #10056, #3623, #5995, #5271, #2781, #10004, #450, #3521, #9144, #5161, #6742, #4466, #5209, #4258, #8456, #1188, #7657, #7503, #4415, #8410, #245, #2730, #9198, #1937, #2677, #396, #6852, #10107, #9300, #1241, #7715, #3675, #6903, #10157, #2882, #6109, #5891, #9358 ),
 .UNSPECIFIED., .F., .T. ) 
 B_SPLINE_CURVE_WITH_KNOTS ( ( 3, 2, 2, 2, 2, 2, 2, 2, 2, 2, 2, 2, 2, 2, 2, 2, 2, 2, 2, 2, 2, 2, 2, 2, 2, 2, 2, 2, 2, 2, 2, 2, 2, 2, 2, 2, 2, 2, 2, 2, 2, 2, 2, 2, 2, 2, 2, 2, 2, 2, 3 ),
 ( 0.000000000000000000, 0.02000000000000000042, 0.04000000000000000083, 0.05999999999999999778, 0.08000000000000000167, 0.1000000000000000056, 0.1199999999999999956, 0.1400000000000000133, 0.1600000000000000033, 0.1799999999999999933, 0.2000000000000000111, 0.2200000000000000011, 0.2399999999999999911, 0.2600000000000000089, 0.2800000000000000266, 0.2999999999999999889, 0.3200000000000000067, 0.3400000000000000244, 0.3599999999999999867, 0.3800000000000000044, 0.4000000000000000222, 0.4199999999999999845, 0.4400000000000000022, 0.4600000000000000200, 0.4799999999999999822, 0.5000000000000000000, 0.5200000000000000178, 0.5400000000000000355, 0.5600000000000000533, 0.5799999999999999600, 0.5999999999999999778, 0.6199999999999999956, 0.6400000000000000133, 0.6600000000000000311, 0.6800000000000000488, 0.6999999999999999556, 0.7199999999999999734, 0.7399999999999999911, 0.7600000000000000089, 0.7800000000000000266, 0.8000000000000000444, 0.8199999999999999512, 0.8399999999999999689, 0.8599999999999999867, 0.8800000000000000044, 0.9000000000000000222, 0.9200000000000000400, 0.9399999999999999467, 0.9599999999999999645, 0.9799999999999999822, 1.000000000000000000 ),
 .UNSPECIFIED. ) 
 CURVE ( )  GEOMETRIC_REPRESENTATION_ITEM ( )  RATIONAL_B_SPLINE_CURVE ( ( 1.000000000000000000, 0.9510565162951535312, 1.000000000000000000, 0.9510565162951535312, 1.000000000000000000, 0.9510565162951535312, 1.000000000000000000, 0.9510565162951535312, 1.000000000000000000, 0.9510565162951535312, 1.000000000000000000, 0.9510565162951535312, 1.000000000000000000, 0.9510565162951535312, 1.000000000000000000, 0.9510565162951535312, 1.000000000000000000, 0.9510565162951535312, 1.000000000000000000, 0.9510565162951535312, 1.000000000000000000, 0.9510565162951535312, 1.000000000000000000, 0.9510565162951535312, 1.000000000000000000, 0.9510565162951535312, 1.000000000000000000, 0.9510565162951535312, 1.000000000000000000, 0.9510565162951535312, 1.000000000000000000, 0.9510565162951535312, 1.000000000000000000, 0.9510565162951535312, 1.000000000000000000, 0.9510565162951535312, 1.000000000000000000, 0.9510565162951535312, 1.000000000000000000, 0.9510565162951535312, 1.000000000000000000, 0.9510565162951535312, 1.000000000000000000, 0.9510565162951535312, 1.000000000000000000, 0.9510565162951535312, 1.000000000000000000, 0.9510565162951535312, 1.000000000000000000, 0.9510565162951535312, 1.000000000000000000, 0.9510565162951535312, 1.000000000000000000, 0.9510565162951535312, 1.000000000000000000, 0.9510565162951535312, 1.000000000000000000, 0.9510565162951535312, 1.000000000000000000, 0.9510565162951535312, 1.000000000000000000, 0.9510565162951535312, 1.000000000000000000, 0.9510565162951535312, 1.000000000000000000, 0.9510565162951535312, 1.000000000000000000, 0.9510565162951535312, 1.000000000000000000, 0.9510565162951535312, 1.000000000000000000, 0.9510565162951535312, 1.000000000000000000, 0.9510565162951535312, 1.000000000000000000, 0.9510565162951535312, 1.000000000000000000, 0.9510565162951535312, 1.000000000000000000, 0.9510565162951535312, 1.000000000000000000, 0.9510565162951535312, 1.000000000000000000, 0.9510565162951535312, 1.000000000000000000, 0.9510565162951535312, 1.000000000000000000, 0.9510565162951535312, 1.000000000000000000, 0.9510565162951535312, 1.000000000000000000, 0.9510565162951535312, 1.000000000000000000, 0.9510565162951535312, 1.000000000000000000, 0.9510565162951535312, 1.000000000000000000, 0.9510565162951535312, 1.000000000000000000, 0.9510565162951535312, 1.000000000000000000 ) ) 
 REPRESENTATION_ITEM ( '' )  );
#5356 = CARTESIAN_POINT ( 'NONE',  ( -0.6146835312500006365, -14.06466310670085562, -1.510416667349463227 ) ) ;
#5357 = EDGE_CURVE ( 'NONE', #5372, #6021, #3669, .T. ) ;
#5358 = CARTESIAN_POINT ( 'NONE',  ( -3.969226411068985882, 2.122056237541205537, 12.16394828327797661 ) ) ;
#5359 = CARTESIAN_POINT ( 'NONE',  ( -0.6146835312500006365, -14.06466310670085562, -1.385416667349463227 ) ) ;
#5360 = ORIENTED_EDGE ( 'NONE', *, *, #5004, .F. ) ;
#5361 = CARTESIAN_POINT ( 'NONE',  ( -0.7500000000000007772, -14.29903810567666156, -2.229166668032259935 ) ) ;
#5362 = DIRECTION ( 'NONE',  ( 0.000000000000000000, 0.000000000000000000, 1.000000000000000000 ) ) ;
#5363 = DIRECTION ( 'NONE',  ( 0.000000000000000000, 0.000000000000000000, 1.000000000000000000 ) ) ;
#5364 = DIRECTION ( 'NONE',  ( 0.9396926207859105373, -0.3420201433256627732, 0.000000000000000000 ) ) ;
#5365 = ORIENTED_EDGE ( 'NONE', *, *, #4095, .T. ) ;
#5366 = EDGE_CURVE ( 'NONE', #1248, #376, #491, .T. ) ;
#5367 = PLANE ( 'NONE',  #2533 ) ;
#5368 = LINE ( 'NONE', #7117, #4744 ) ;
#5369 = CARTESIAN_POINT ( 'NONE',  ( -0.7401821875142701179, 4.673326407553649808, 5.179999999999999716 ) ) ;
#5370 = CARTESIAN_POINT ( 'NONE',  ( -1.229367062500000385, -13.70977540446723886, -0.05208333401612993269 ) ) ;
#5371 = ORIENTED_EDGE ( 'NONE', *, *, #1152, .T. ) ;
#5372 = VERTEX_POINT ( 'NONE', #3141 ) ;
#5373 = DIRECTION ( 'NONE',  ( -1.000000000000000000, -1.156482317317871478E-16, -5.637851296924623057E-15 ) ) ;
#5374 = LINE ( 'NONE', #8614, #7288 ) ;
#5375 = ORIENTED_EDGE ( 'NONE', *, *, #6053, .T. ) ;
#5376 = EDGE_CURVE ( 'NONE', #216, #7456, #6368, .T. ) ;
#5377 = CARTESIAN_POINT ( 'NONE',  ( 4.155232146225751322, -4.023224611898307934, 10.09605171672202140 ) ) ;
#5378 = EDGE_CURVE ( 'NONE', #6291, #307, #8130, .T. ) ;
#5379 = CARTESIAN_POINT ( 'NONE',  ( 15.00000000000000000, 19.99999999999999645, -9.000000000000000000 ) ) ;
#5380 = ORIENTED_EDGE ( 'NONE', *, *, #3838, .T. ) ;
#5381 = CARTESIAN_POINT ( 'NONE',  ( 23.25451694676619496, 6.000000000000000000, -12.00000000000000000 ) ) ;
#5382 = ORIENTED_EDGE ( 'NONE', *, *, #6829, .T. ) ;
#5383 = SURFACE_STYLE_USAGE ( .BOTH. , #2214 ) ;
#5384 = ORIENTED_EDGE ( 'NONE', *, *, #6615, .T. ) ;
#5385 = CARTESIAN_POINT ( 'NONE',  ( 7.546553696766196140, 6.000000000000000000, -12.00000000000000000 ) ) ;
#5386 = VECTOR ( 'NONE', #4555, 1000.000000000000000 ) ;
#5387 = DIRECTION ( 'NONE',  ( -0.000000000000000000, 1.000000000000000000, -0.000000000000000000 ) ) ;
#5388 = VERTEX_POINT ( 'NONE', #3296 ) ;
#5389 = EDGE_CURVE ( 'NONE', #2210, #6021, #4093, .T. ) ;
#5390 = CARTESIAN_POINT ( 'NONE',  ( 0.000000000000000000, -7.750000000000000000, -12.00000000000000000 ) ) ;
#5391 = PLANE ( 'NONE',  #9884 ) ;
#5392 = CARTESIAN_POINT ( 'NONE',  ( -0.9480714621563718358, -5.418398423912716311, 8.523948283277976046 ) ) ;
#5393 = ORIENTED_EDGE ( 'NONE', *, *, #5886, .T. ) ;
#5394 = LINE ( 'NONE', #578, #6942 ) ;
#5395 = FACE_OUTER_BOUND ( 'NONE', #1941, .T. ) ;
#5396 = CARTESIAN_POINT ( 'NONE',  ( -2.000000000000000000, 0.000000000000000000, 0.000000000000000000 ) ) ;
#5397 = CIRCLE ( 'NONE', #6241, 1.249999999999997558 ) ;
#5398 = CARTESIAN_POINT ( 'NONE',  ( -2.000000000000000000, 3.771202944355774189, -4.982773259188334691 ) ) ;
#5399 = CARTESIAN_POINT ( 'NONE',  ( -2.000000000000000000, 1.459547570502460978, -6.894905428400257996 ) ) ;
#5400 = DIRECTION ( 'NONE',  ( 1.000000000000000000, 0.000000000000000000, 0.000000000000000000 ) ) ;
#5401 = EDGE_CURVE ( 'NONE', #8892, #9635, #6775, .T. ) ;
#5402 = CARTESIAN_POINT ( 'NONE',  ( -3.181725716174720991E-16, -14.73205080756888563, -1.125000000000000222 ) ) ;
#5403 = VECTOR ( 'NONE', #9173, 1000.000000000000000 ) ;
#5404 = DIRECTION ( 'NONE',  ( 0.000000000000000000, -0.000000000000000000, 1.000000000000000000 ) ) ;
#5405 = CARTESIAN_POINT ( 'NONE',  ( -2.042957248827969252, 4.009529358847651714, 5.039999999999999147 ) ) ;
#5406 = MECHANICAL_DESIGN_GEOMETRIC_PRESENTATION_REPRESENTATION (  '', ( #6249 ), #3047 ) ;
#5407 = CARTESIAN_POINT ( 'NONE',  ( -0.6146835312499998594, -11.93533689329915326, -2.677083334016129967 ) ) ;
#5408 = CARTESIAN_POINT ( 'NONE',  ( -4.023224611898323033, 4.155232146225737111, 12.30394828327797718 ) ) ;
#5409 = FACE_OUTER_BOUND ( 'NONE', #5499, .T. ) ;
#5410 = ORIENTED_EDGE ( 'NONE', *, *, #4455, .F. ) ;
#5411 = AXIS2_PLACEMENT_3D ( 'NONE', #3864, #9392, #9502 ) ;
#5412 = CARTESIAN_POINT ( 'NONE',  ( 20.72778015323380885, 6.000000000000000000, 0.000000000000000000 ) ) ;
#5413 =( BOUNDED_SURFACE ( )  B_SPLINE_SURFACE ( 3, 2, ( 
 ( #9544, #1690, #4968, #2435, #7196, #3278, #4916, #3221, #7249, #3300, #4120, #6500, #8213, #2590, #5700, #9758, #6607, #9864, #6554, #10453, #2487, #8164, #6451, #9708, #5654, #7359, #8946, #947, #5805, #894, #102, #9057, #1795, #9807, #3329, #2536, #5755, #9004, #1741, #7408, #149, #8898, #4173, #3380, #8003, #1640, #4020, #735, #2378, #3967, #3170, #4862, #6394, #9651, #8107, #839, #5605, #4070, #8848, #1589, #4811, #7307, #49, #8059, #790, #4271, #10019, #9262, #3586, #6009, #5857, #8368, #7465, #3636, #5955, #6866, #9109, #2002, #10120, #5068, #9313, #1097, #308, #2640, #5221, #8471, #1845, #1949, #5172, #9210, #6811, #1203, #8421, #4427, #2842, #208, #4222, #5907, #1147, #4370, #6058 ),
 ( #2791, #2688, #7516, #4321, #7617, #8320, #7672, #3432, #360, #5023, #410, #8267, #992, #3484, #10067, #6655, #9912, #1050, #257, #6707, #9965, #5120, #9160, #1900, #7565, #3531, #6757, #2744, #2055, #2208, #6328, #2105, #6118, #7773, #10383, #9475, #2156, #4479, #506, #6219, #9533, #6968, #1464, #4687, #3739, #7019, #8722, #5281, #1303, #8573, #7071, #6913, #3106, #2260, #10222, #1254, #7727, #2952, #6171, #460, #9427, #3687, #6277, #5483, #1355, #5377, #8616, #10169, #4529, #10275, #7931, #615, #3055, #2897, #4583, #9370, #663, #3004, #3897, #5330, #7127, #8522, #7829, #561, #3789, #5435, #8673, #1407, #4632, #7879, #3843, #10320, #178, #8292, #3460, #9888, #9942, #1075, #4889, #8777, #128 ),
 ( #8190, #235, #76, #1821, #3303, #2617, #2666, #919, #3511, #5834, #9087, #6530, #5881, #8978, #8138, #4148, #9783, #6683, #4248, #8244, #1769, #5044, #7434, #9130, #4998, #7385, #1873, #2512, #5726, #6580, #1721, #5098, #5781, #5536, #3412, #2567, #1019, #1518, #4297, #9032, #4945, #3353, #873, #971, #9837, #7493, #4197, #7542, #9586, #7333, #8346, #4100, #6635, #286, #2313, #2026, #5199, #6727, #8444, #8596, #3664, #1327, #2133, #7589, #3611, #1979, #8396, #6838, #1281, #9187, #7648, #1174, #385, #10199, #9990, #6892, #539, #6789, #332, #4402, #4556, #10145, #10095, #1925, #2822, #438, #3712, #6035, #5935, #5256, #2868, #9287, #5982, #9240, #6092, #8497, #6944, #7805, #4453, #1228, #5354 ),
 ( #7701, #9346, #4507, #6146, #9396, #2080, #5306, #2927, #2716, #8547, #2769, #7752, #1127, #5148, #4348, #486, #3561, #10046, #2238, #8698, #9452, #638, #6199, #8018, #751, #3082, #3868, #7907, #2181, #3027, #8752, #3984, #2340, #4773, #4609, #7100, #5405, #2397, #4711, #5617, #7851, #7215, #8861, #3818, #8073, #10358, #9561, #1385, #10468, #3185, #587, #699, #3928, #7962, #5562, #6407, #7155, #9667, #1603, #8649, #2980, #4661, #10412, #3133, #4826, #3764, #6995, #5459, #6302, #1551, #1435, #6248, #2288, #6361, #7047, #10247, #10299, #9613, #9508, #5512, #1491, #8807, #9773, #3396, #3240, #6625, #7421, #5084, #4237, #9018, #4134, #164, #7261, #5871, #7373, #4087, #8121, #6463, #3341, #8961, #5822 ),
 ( #64, #3290, #9876, #9820, #8281, #9121, #1756, #2552, #9929, #2656, #2606, #5769, #9075, #4983, #6569, #1810, #223, #3448, #2501, #8230, #7483, #804, #6516, #7321, #5035, #5665, #1861, #1007, #1704, #9, #9720, #5714, #4933, #2451, #8176, #8914, #6671, #4032, #117, #908, #961, #1652, #4187, #4877, #855, #6881, #9334, #9177, #1161, #273, #6927, #9276, #10187, #1915, #2070, #2915, #8383, #2119, #4388, #3600, #5921, #5294, #8536, #5137, #5241, #8486, #2015, #10135, #1268, #1218, #4495, #6132, #3500, #7528, #9226, #4441, #7689, #9384, #8337, #7740, #10036, #7635, #6078, #5972, #321, #375, #425, #1113, #475, #6717, #3654, #1064, #3699, #4287, #9978, #6773, #2856, #2702, #4338, #7578, #3548 ),
 ( #2757, #1966, #5188, #8435, #6826, #10083, #2810, #6025, #575, #4763, #8793, #3803, #1477, #8005, #738, #3017, #2966, #6234, #6290, #3969, #8740, #2328, #4542, #10236, #4699, #9546, #8686, #7086, #7198, #3858, #7945, #3119, #10455, #4596, #7788, #3172, #682, #5550, #7036, #3915, #5446, #6397, #1422, #9600, #2274, #7839, #524, #10400, #4649, #8586, #6346, #10287, #7141, #6187, #5344, #1371, #7895, #3752, #629, #1535, #9493, #9653, #1317, #9441, #6983, #2169, #2226, #10341, #5392, #8633, #3071, #5498, #3382, #3223, #4970, #6453, #2538, #2593, #4072, #6657, #5757, #9006, #9710, #9060, #1642, #792, #841, #2437, #9865, #7410, #896, #4918, #8216, #104, #6610, #8166, #7309, #5025, #5656, #8901, #9760 ),
 ( #3331, #5702, #1743, #8850, #7468, #8948, #4864, #8109, #4814, #4122, #51, #152, #3280, #210, #2380, #1786, #949, #7251, #7362, #4022, #5807, #6557, #6503, #5607, #2490, #4225, #9809, #3434, #8269, #1692, #4175, #1797, #994, #1591, #8061, #1256, #8423, #9264, #7674, #5283, #9164, #9111, #9316, #5225, #6868, #5122, #2004, #10022, #7730, #2746, #3640, #363, #1903, #1847, #4429, #5958, #2643, #412, #8370, #1206, #7518, #9915, #5909, #9212, #8324, #1952, #8473, #1099, #10122, #2844, #4273, #6061, #2058, #4323, #5174, #3689, #6709, #4481, #7567, #8524, #261, #462, #3487, #10070, #5859, #310, #5070, #2795, #6011, #9967, #1052, #3534, #2690, #6759, #1149, #4373, #7619, #3588, #6813, #2261, #4634 ) ),
 .UNSPECIFIED., .T., .F., .T. ) 
 B_SPLINE_SURFACE_WITH_KNOTS ( ( 4, 3, 4 ),
 ( 3, 2, 2, 2, 2, 2, 2, 2, 2, 2, 2, 2, 2, 2, 2, 2, 2, 2, 2, 2, 2, 2, 2, 2, 2, 2, 2, 2, 2, 2, 2, 2, 2, 2, 2, 2, 2, 2, 2, 2, 2, 2, 2, 2, 2, 2, 2, 2, 2, 2, 3 ),
 ( 0.000000000000000000, 0.5000000000000000000, 1.000000000000000000 ),
 ( 0.000000000000000000, 0.02000000000000000042, 0.04000000000000000083, 0.05999999999999999778, 0.08000000000000000167, 0.1000000000000000056, 0.1199999999999999956, 0.1400000000000000133, 0.1600000000000000033, 0.1799999999999999933, 0.2000000000000000111, 0.2200000000000000011, 0.2399999999999999911, 0.2600000000000000089, 0.2800000000000000266, 0.2999999999999999889, 0.3200000000000000067, 0.3400000000000000244, 0.3599999999999999867, 0.3800000000000000044, 0.4000000000000000222, 0.4199999999999999845, 0.4400000000000000022, 0.4600000000000000200, 0.4799999999999999822, 0.5000000000000000000, 0.5200000000000000178, 0.5400000000000000355, 0.5600000000000000533, 0.5799999999999999600, 0.5999999999999999778, 0.6199999999999999956, 0.6400000000000000133, 0.6600000000000000311, 0.6800000000000000488, 0.6999999999999999556, 0.7199999999999999734, 0.7399999999999999911, 0.7600000000000000089, 0.7800000000000000266, 0.8000000000000000444, 0.8199999999999999512, 0.8399999999999999689, 0.8599999999999999867, 0.8800000000000000044, 0.9000000000000000222, 0.9200000000000000400, 0.9399999999999999467, 0.9599999999999999645, 0.9799999999999999822, 1.000000000000000000 ),
 .UNSPECIFIED. ) 
 GEOMETRIC_REPRESENTATION_ITEM ( )  RATIONAL_B_SPLINE_SURFACE ( (
 ( 1.000000000000000000, 0.9510565162951535312, 1.000000000000000000, 0.9510565162951535312, 1.000000000000000000, 0.9510565162951535312, 1.000000000000000000, 0.9510565162951535312, 1.000000000000000000, 0.9510565162951535312, 1.000000000000000000, 0.9510565162951535312, 1.000000000000000000, 0.9510565162951535312, 1.000000000000000000, 0.9510565162951535312, 1.000000000000000000, 0.9510565162951535312, 1.000000000000000000, 0.9510565162951535312, 1.000000000000000000, 0.9510565162951535312, 1.000000000000000000, 0.9510565162951535312, 1.000000000000000000, 0.9510565162951535312, 1.000000000000000000, 0.9510565162951535312, 1.000000000000000000, 0.9510565162951535312, 1.000000000000000000, 0.9510565162951535312, 1.000000000000000000, 0.9510565162951535312, 1.000000000000000000, 0.9510565162951535312, 1.000000000000000000, 0.9510565162951535312, 1.000000000000000000, 0.9510565162951535312, 1.000000000000000000, 0.9510565162951535312, 1.000000000000000000, 0.9510565162951535312, 1.000000000000000000, 0.9510565162951535312, 1.000000000000000000, 0.9510565162951535312, 1.000000000000000000, 0.9510565162951535312, 1.000000000000000000, 0.9510565162951535312, 1.000000000000000000, 0.9510565162951535312, 1.000000000000000000, 0.9510565162951535312, 1.000000000000000000, 0.9510565162951535312, 1.000000000000000000, 0.9510565162951535312, 1.000000000000000000, 0.9510565162951535312, 1.000000000000000000, 0.9510565162951535312, 1.000000000000000000, 0.9510565162951535312, 1.000000000000000000, 0.9510565162951535312, 1.000000000000000000, 0.9510565162951535312, 1.000000000000000000, 0.9510565162951535312, 1.000000000000000000, 0.9510565162951535312, 1.000000000000000000, 0.9510565162951535312, 1.000000000000000000, 0.9510565162951535312, 1.000000000000000000, 0.9510565162951535312, 1.000000000000000000, 0.9510565162951535312, 1.000000000000000000, 0.9510565162951535312, 1.000000000000000000, 0.9510565162951535312, 1.000000000000000000, 0.9510565162951535312, 1.000000000000000000, 0.9510565162951535312, 1.000000000000000000, 0.9510565162951535312, 1.000000000000000000, 0.9510565162951535312, 1.000000000000000000, 0.9510565162951535312, 1.000000000000000000, 0.9510565162951535312, 1.000000000000000000, 0.9510565162951535312, 1.000000000000000000),
 ( 0.3333333333333333703, 0.3170188387650512141, 0.3333333333333333703, 0.3170188387650512141, 0.3333333333333333703, 0.3170188387650512141, 0.3333333333333333703, 0.3170188387650512141, 0.3333333333333333703, 0.3170188387650512141, 0.3333333333333333703, 0.3170188387650512141, 0.3333333333333333703, 0.3170188387650512141, 0.3333333333333333703, 0.3170188387650512141, 0.3333333333333333703, 0.3170188387650512141, 0.3333333333333333703, 0.3170188387650512141, 0.3333333333333333703, 0.3170188387650512141, 0.3333333333333333703, 0.3170188387650512141, 0.3333333333333333703, 0.3170188387650512141, 0.3333333333333333703, 0.3170188387650512141, 0.3333333333333333703, 0.3170188387650512141, 0.3333333333333333703, 0.3170188387650512141, 0.3333333333333333703, 0.3170188387650512141, 0.3333333333333333703, 0.3170188387650512141, 0.3333333333333333703, 0.3170188387650512141, 0.3333333333333333703, 0.3170188387650512141, 0.3333333333333333703, 0.3170188387650512141, 0.3333333333333333703, 0.3170188387650512141, 0.3333333333333333703, 0.3170188387650512141, 0.3333333333333333703, 0.3170188387650512141, 0.3333333333333333703, 0.3170188387650512141, 0.3333333333333333703, 0.3170188387650512141, 0.3333333333333333703, 0.3170188387650512141, 0.3333333333333333703, 0.3170188387650512141, 0.3333333333333333703, 0.3170188387650512141, 0.3333333333333333703, 0.3170188387650512141, 0.3333333333333333703, 0.3170188387650512141, 0.3333333333333333703, 0.3170188387650512141, 0.3333333333333333703, 0.3170188387650512141, 0.3333333333333333703, 0.3170188387650512141, 0.3333333333333333703, 0.3170188387650512141, 0.3333333333333333703, 0.3170188387650512141, 0.3333333333333333703, 0.3170188387650512141, 0.3333333333333333703, 0.3170188387650512141, 0.3333333333333333703, 0.3170188387650512141, 0.3333333333333333703, 0.3170188387650512141, 0.3333333333333333703, 0.3170188387650512141, 0.3333333333333333703, 0.3170188387650512141, 0.3333333333333333703, 0.3170188387650512141, 0.3333333333333333703, 0.3170188387650512141, 0.3333333333333333703, 0.3170188387650512141, 0.3333333333333333703, 0.3170188387650512141, 0.3333333333333333703, 0.3170188387650512141, 0.3333333333333333703, 0.3170188387650512141, 0.3333333333333333703, 0.3170188387650512141, 0.3333333333333333703, 0.3170188387650512141, 0.3333333333333333703),
 ( 0.3333333333333333703, 0.3170188387650512141, 0.3333333333333333703, 0.3170188387650512141, 0.3333333333333333703, 0.3170188387650512141, 0.3333333333333333703, 0.3170188387650512141, 0.3333333333333333703, 0.3170188387650512141, 0.3333333333333333703, 0.3170188387650512141, 0.3333333333333333703, 0.3170188387650512141, 0.3333333333333333703, 0.3170188387650512141, 0.3333333333333333703, 0.3170188387650512141, 0.3333333333333333703, 0.3170188387650512141, 0.3333333333333333703, 0.3170188387650512141, 0.3333333333333333703, 0.3170188387650512141, 0.3333333333333333703, 0.3170188387650512141, 0.3333333333333333703, 0.3170188387650512141, 0.3333333333333333703, 0.3170188387650512141, 0.3333333333333333703, 0.3170188387650512141, 0.3333333333333333703, 0.3170188387650512141, 0.3333333333333333703, 0.3170188387650512141, 0.3333333333333333703, 0.3170188387650512141, 0.3333333333333333703, 0.3170188387650512141, 0.3333333333333333703, 0.3170188387650512141, 0.3333333333333333703, 0.3170188387650512141, 0.3333333333333333703, 0.3170188387650512141, 0.3333333333333333703, 0.3170188387650512141, 0.3333333333333333703, 0.3170188387650512141, 0.3333333333333333703, 0.3170188387650512141, 0.3333333333333333703, 0.3170188387650512141, 0.3333333333333333703, 0.3170188387650512141, 0.3333333333333333703, 0.3170188387650512141, 0.3333333333333333703, 0.3170188387650512141, 0.3333333333333333703, 0.3170188387650512141, 0.3333333333333333703, 0.3170188387650512141, 0.3333333333333333703, 0.3170188387650512141, 0.3333333333333333703, 0.3170188387650512141, 0.3333333333333333703, 0.3170188387650512141, 0.3333333333333333703, 0.3170188387650512141, 0.3333333333333333703, 0.3170188387650512141, 0.3333333333333333703, 0.3170188387650512141, 0.3333333333333333703, 0.3170188387650512141, 0.3333333333333333703, 0.3170188387650512141, 0.3333333333333333703, 0.3170188387650512141, 0.3333333333333333703, 0.3170188387650512141, 0.3333333333333333703, 0.3170188387650512141, 0.3333333333333333703, 0.3170188387650512141, 0.3333333333333333703, 0.3170188387650512141, 0.3333333333333333703, 0.3170188387650512141, 0.3333333333333333703, 0.3170188387650512141, 0.3333333333333333703, 0.3170188387650512141, 0.3333333333333333703, 0.3170188387650512141, 0.3333333333333333703, 0.3170188387650512141, 0.3333333333333333703),
 ( 1.000000000000000000, 0.9510565162951535312, 1.000000000000000000, 0.9510565162951535312, 1.000000000000000000, 0.9510565162951535312, 1.000000000000000000, 0.9510565162951535312, 1.000000000000000000, 0.9510565162951535312, 1.000000000000000000, 0.9510565162951535312, 1.000000000000000000, 0.9510565162951535312, 1.000000000000000000, 0.9510565162951535312, 1.000000000000000000, 0.9510565162951535312, 1.000000000000000000, 0.9510565162951535312, 1.000000000000000000, 0.9510565162951535312, 1.000000000000000000, 0.9510565162951535312, 1.000000000000000000, 0.9510565162951535312, 1.000000000000000000, 0.9510565162951535312, 1.000000000000000000, 0.9510565162951535312, 1.000000000000000000, 0.9510565162951535312, 1.000000000000000000, 0.9510565162951535312, 1.000000000000000000, 0.9510565162951535312, 1.000000000000000000, 0.9510565162951535312, 1.000000000000000000, 0.9510565162951535312, 1.000000000000000000, 0.9510565162951535312, 1.000000000000000000, 0.9510565162951535312, 1.000000000000000000, 0.9510565162951535312, 1.000000000000000000, 0.9510565162951535312, 1.000000000000000000, 0.9510565162951535312, 1.000000000000000000, 0.9510565162951535312, 1.000000000000000000, 0.9510565162951535312, 1.000000000000000000, 0.9510565162951535312, 1.000000000000000000, 0.9510565162951535312, 1.000000000000000000, 0.9510565162951535312, 1.000000000000000000, 0.9510565162951535312, 1.000000000000000000, 0.9510565162951535312, 1.000000000000000000, 0.9510565162951535312, 1.000000000000000000, 0.9510565162951535312, 1.000000000000000000, 0.9510565162951535312, 1.000000000000000000, 0.9510565162951535312, 1.000000000000000000, 0.9510565162951535312, 1.000000000000000000, 0.9510565162951535312, 1.000000000000000000, 0.9510565162951535312, 1.000000000000000000, 0.9510565162951535312, 1.000000000000000000, 0.9510565162951535312, 1.000000000000000000, 0.9510565162951535312, 1.000000000000000000, 0.9510565162951535312, 1.000000000000000000, 0.9510565162951535312, 1.000000000000000000, 0.9510565162951535312, 1.000000000000000000, 0.9510565162951535312, 1.000000000000000000, 0.9510565162951535312, 1.000000000000000000, 0.9510565162951535312, 1.000000000000000000, 0.9510565162951535312, 1.000000000000000000, 0.9510565162951535312, 1.000000000000000000),
 ( 0.3333333333333333703, 0.3170188387650512141, 0.3333333333333333703, 0.3170188387650512141, 0.3333333333333333703, 0.3170188387650512141, 0.3333333333333333703, 0.3170188387650512141, 0.3333333333333333703, 0.3170188387650512141, 0.3333333333333333703, 0.3170188387650512141, 0.3333333333333333703, 0.3170188387650512141, 0.3333333333333333703, 0.3170188387650512141, 0.3333333333333333703, 0.3170188387650512141, 0.3333333333333333703, 0.3170188387650512141, 0.3333333333333333703, 0.3170188387650512141, 0.3333333333333333703, 0.3170188387650512141, 0.3333333333333333703, 0.3170188387650512141, 0.3333333333333333703, 0.3170188387650512141, 0.3333333333333333703, 0.3170188387650512141, 0.3333333333333333703, 0.3170188387650512141, 0.3333333333333333703, 0.3170188387650512141, 0.3333333333333333703, 0.3170188387650512141, 0.3333333333333333703, 0.3170188387650512141, 0.3333333333333333703, 0.3170188387650512141, 0.3333333333333333703, 0.3170188387650512141, 0.3333333333333333703, 0.3170188387650512141, 0.3333333333333333703, 0.3170188387650512141, 0.3333333333333333703, 0.3170188387650512141, 0.3333333333333333703, 0.3170188387650512141, 0.3333333333333333703, 0.3170188387650512141, 0.3333333333333333703, 0.3170188387650512141, 0.3333333333333333703, 0.3170188387650512141, 0.3333333333333333703, 0.3170188387650512141, 0.3333333333333333703, 0.3170188387650512141, 0.3333333333333333703, 0.3170188387650512141, 0.3333333333333333703, 0.3170188387650512141, 0.3333333333333333703, 0.3170188387650512141, 0.3333333333333333703, 0.3170188387650512141, 0.3333333333333333703, 0.3170188387650512141, 0.3333333333333333703, 0.3170188387650512141, 0.3333333333333333703, 0.3170188387650512141, 0.3333333333333333703, 0.3170188387650512141, 0.3333333333333333703, 0.3170188387650512141, 0.3333333333333333703, 0.3170188387650512141, 0.3333333333333333703, 0.3170188387650512141, 0.3333333333333333703, 0.3170188387650512141, 0.3333333333333333703, 0.3170188387650512141, 0.3333333333333333703, 0.3170188387650512141, 0.3333333333333333703, 0.3170188387650512141, 0.3333333333333333703, 0.3170188387650512141, 0.3333333333333333703, 0.3170188387650512141, 0.3333333333333333703, 0.3170188387650512141, 0.3333333333333333703, 0.3170188387650512141, 0.3333333333333333703, 0.3170188387650512141, 0.3333333333333333703),
 ( 0.3333333333333333703, 0.3170188387650512141, 0.3333333333333333703, 0.3170188387650512141, 0.3333333333333333703, 0.3170188387650512141, 0.3333333333333333703, 0.3170188387650512141, 0.3333333333333333703, 0.3170188387650512141, 0.3333333333333333703, 0.3170188387650512141, 0.3333333333333333703, 0.3170188387650512141, 0.3333333333333333703, 0.3170188387650512141, 0.3333333333333333703, 0.3170188387650512141, 0.3333333333333333703, 0.3170188387650512141, 0.3333333333333333703, 0.3170188387650512141, 0.3333333333333333703, 0.3170188387650512141, 0.3333333333333333703, 0.3170188387650512141, 0.3333333333333333703, 0.3170188387650512141, 0.3333333333333333703, 0.3170188387650512141, 0.3333333333333333703, 0.3170188387650512141, 0.3333333333333333703, 0.3170188387650512141, 0.3333333333333333703, 0.3170188387650512141, 0.3333333333333333703, 0.3170188387650512141, 0.3333333333333333703, 0.3170188387650512141, 0.3333333333333333703, 0.3170188387650512141, 0.3333333333333333703, 0.3170188387650512141, 0.3333333333333333703, 0.3170188387650512141, 0.3333333333333333703, 0.3170188387650512141, 0.3333333333333333703, 0.3170188387650512141, 0.3333333333333333703, 0.3170188387650512141, 0.3333333333333333703, 0.3170188387650512141, 0.3333333333333333703, 0.3170188387650512141, 0.3333333333333333703, 0.3170188387650512141, 0.3333333333333333703, 0.3170188387650512141, 0.3333333333333333703, 0.3170188387650512141, 0.3333333333333333703, 0.3170188387650512141, 0.3333333333333333703, 0.3170188387650512141, 0.3333333333333333703, 0.3170188387650512141, 0.3333333333333333703, 0.3170188387650512141, 0.3333333333333333703, 0.3170188387650512141, 0.3333333333333333703, 0.3170188387650512141, 0.3333333333333333703, 0.3170188387650512141, 0.3333333333333333703, 0.3170188387650512141, 0.3333333333333333703, 0.3170188387650512141, 0.3333333333333333703, 0.3170188387650512141, 0.3333333333333333703, 0.3170188387650512141, 0.3333333333333333703, 0.3170188387650512141, 0.3333333333333333703, 0.3170188387650512141, 0.3333333333333333703, 0.3170188387650512141, 0.3333333333333333703, 0.3170188387650512141, 0.3333333333333333703, 0.3170188387650512141, 0.3333333333333333703, 0.3170188387650512141, 0.3333333333333333703, 0.3170188387650512141, 0.3333333333333333703, 0.3170188387650512141, 0.3333333333333333703),
 ( 1.000000000000000000, 0.9510565162951535312, 1.000000000000000000, 0.9510565162951535312, 1.000000000000000000, 0.9510565162951535312, 1.000000000000000000, 0.9510565162951535312, 1.000000000000000000, 0.9510565162951535312, 1.000000000000000000, 0.9510565162951535312, 1.000000000000000000, 0.9510565162951535312, 1.000000000000000000, 0.9510565162951535312, 1.000000000000000000, 0.9510565162951535312, 1.000000000000000000, 0.9510565162951535312, 1.000000000000000000, 0.9510565162951535312, 1.000000000000000000, 0.9510565162951535312, 1.000000000000000000, 0.9510565162951535312, 1.000000000000000000, 0.9510565162951535312, 1.000000000000000000, 0.9510565162951535312, 1.000000000000000000, 0.9510565162951535312, 1.000000000000000000, 0.9510565162951535312, 1.000000000000000000, 0.9510565162951535312, 1.000000000000000000, 0.9510565162951535312, 1.000000000000000000, 0.9510565162951535312, 1.000000000000000000, 0.9510565162951535312, 1.000000000000000000, 0.9510565162951535312, 1.000000000000000000, 0.9510565162951535312, 1.000000000000000000, 0.9510565162951535312, 1.000000000000000000, 0.9510565162951535312, 1.000000000000000000, 0.9510565162951535312, 1.000000000000000000, 0.9510565162951535312, 1.000000000000000000, 0.9510565162951535312, 1.000000000000000000, 0.9510565162951535312, 1.000000000000000000, 0.9510565162951535312, 1.000000000000000000, 0.9510565162951535312, 1.000000000000000000, 0.9510565162951535312, 1.000000000000000000, 0.9510565162951535312, 1.000000000000000000, 0.9510565162951535312, 1.000000000000000000, 0.9510565162951535312, 1.000000000000000000, 0.9510565162951535312, 1.000000000000000000, 0.9510565162951535312, 1.000000000000000000, 0.9510565162951535312, 1.000000000000000000, 0.9510565162951535312, 1.000000000000000000, 0.9510565162951535312, 1.000000000000000000, 0.9510565162951535312, 1.000000000000000000, 0.9510565162951535312, 1.000000000000000000, 0.9510565162951535312, 1.000000000000000000, 0.9510565162951535312, 1.000000000000000000, 0.9510565162951535312, 1.000000000000000000, 0.9510565162951535312, 1.000000000000000000, 0.9510565162951535312, 1.000000000000000000, 0.9510565162951535312, 1.000000000000000000, 0.9510565162951535312, 1.000000000000000000, 0.9510565162951535312, 1.000000000000000000) ) ) 
 REPRESENTATION_ITEM ( '' )  SURFACE ( )  );
#5414 = CARTESIAN_POINT ( 'NONE',  ( 23.86937280323380506, 6.000000000000000000, -12.00000000000000000 ) ) ;
#5415 = CARTESIAN_POINT ( 'NONE',  ( 16.15239861966725599, 3.750000000000000000, -12.00000000000000000 ) ) ;
#5416 = CARTESIAN_POINT ( 'NONE',  ( 9.980802115791359341, 9.632714884249118370, 0.000000000000000000 ) ) ;
#5417 = EDGE_LOOP ( 'NONE', ( #8906, #10018, #1442, #6902, #9457 ) ) ;
#5418 = VECTOR ( 'NONE', #1504, 1000.000000000000000 ) ;
#5419 = CARTESIAN_POINT ( 'NONE',  ( 0.7499999999999991118, -14.29903810567666333, -0.1458333346989267310 ) ) ;
#5420 = EDGE_CURVE ( 'NONE', #7594, #7022, #3088, .T. ) ;
#5421 = SURFACE_STYLE_FILL_AREA ( #3095 ) ;
#5422 = VECTOR ( 'NONE', #1659, 1000.000000000000000 ) ;
#5423 = CARTESIAN_POINT ( 'NONE',  ( -2.042957248827969252, 4.009529358847651714, 13.43999999999999950 ) ) ;
#5424 = AXIS2_PLACEMENT_3D ( 'NONE', #1758, #7266, #8178 ) ;
#5425 = CARTESIAN_POINT ( 'NONE',  ( 0.6146835312499993043, -14.06466310670085562, -1.427083334016129967 ) ) ;
#5426 = EDGE_LOOP ( 'NONE', ( #7263, #893 ) ) ;
#5427 = VECTOR ( 'NONE', #3337, 1000.000000000000000 ) ;
#5428 = CIRCLE ( 'NONE', #7642, 2.500000000000000000 ) ;
#5429 = EDGE_CURVE ( 'NONE', #6690, #4861, #6415, .T. ) ;
#5430 = ORIENTED_EDGE ( 'NONE', *, *, #628, .F. ) ;
#5431 = LINE ( 'NONE', #7236, #5927 ) ;
#5432 = VECTOR ( 'NONE', #8727, 1000.000000000000000 ) ;
#5433 = CARTESIAN_POINT ( 'NONE',  ( -1.500000000000000222, -13.00000000000000533, -2.312500001365593860 ) ) ;
#5434 = ORIENTED_EDGE ( 'NONE', *, *, #1388, .T. ) ;
#5435 = CARTESIAN_POINT ( 'NONE',  ( 4.155232146225751322, -4.023224611898307934, 12.89605171672202211 ) ) ;
#5436 = ORIENTED_EDGE ( 'NONE', *, *, #7643, .T. ) ;
#5437 = FACE_OUTER_BOUND ( 'NONE', #3006, .T. ) ;
#5438 = CARTESIAN_POINT ( 'NONE',  ( 5.110351332421769754, 2.708615832122969191, 12.33605171672202339 ) ) ;
#5439 = ORIENTED_EDGE ( 'NONE', *, *, #5557, .F. ) ;
#5440 = ORIENTED_EDGE ( 'NONE', *, *, #2418, .F. ) ;
#5441 = CARTESIAN_POINT ( 'NONE',  ( 1.999999999999973577, 35.00000000000000000, 6.000000000000010658 ) ) ;
#5442 = DIRECTION ( 'NONE',  ( -1.000000000000000000, -0.000000000000000000, 0.000000000000000000 ) ) ;
#5443 = ORIENTED_EDGE ( 'NONE', *, *, #6684, .T. ) ;
#5444 = DIRECTION ( 'NONE',  ( -1.000000000000000000, -0.000000000000000000, -0.000000000000000000 ) ) ;
#5445 = LINE ( 'NONE', #2013, #2109 ) ;
#5446 = CARTESIAN_POINT ( 'NONE',  ( 3.951860609387084722, 3.826313983664940022, 4.603948283277976117 ) ) ;
#5447 = EDGE_LOOP ( 'NONE', ( #630, #10288, #1318, #4163 ) ) ;
#5448 = LINE ( 'NONE', #8488, #1878 ) ;
#5449 = DIRECTION ( 'NONE',  ( -1.000000000000000000, -0.000000000000000000, -0.000000000000000000 ) ) ;
#5450 = EDGE_CURVE ( 'NONE', #10028, #8730, #3875, .T. ) ;
#5451 = DIRECTION ( 'NONE',  ( 0.000000000000000000, 0.000000000000000000, -1.000000000000000000 ) ) ;
#5452 = ADVANCED_FACE ( 'NONE', ( #8080 ), #9622, .F. ) ;
#5453 = PRODUCT ( 'rack_ISO - Rack-spur - rectangular 1M 20PA 12FW 5PH 25L---SAll', 'rack_ISO - Rack-spur - rectangular 1M 20PA 12FW 5PH 25L---SAll', '', ( #9726 ) ) ;
#5454 = FACE_OUTER_BOUND ( 'NONE', #10279, .T. ) ;
#5455 = CARTESIAN_POINT ( 'NONE',  ( 1.060575238724907038E-16, -11.26794919243112680, -2.375000000000000444 ) ) ;
#5456 = FACE_OUTER_BOUND ( 'NONE', #3616, .T. ) ;
#5457 = CARTESIAN_POINT ( 'NONE',  ( -0.7500000000000007772, -14.29903810567666156, -1.166666666666666741 ) ) ;
#5458 = DIRECTION ( 'NONE',  ( 0.3420201433256627732, 0.9396926207859105373, 0.000000000000000000 ) ) ;
#5459 = CARTESIAN_POINT ( 'NONE',  ( 0.7401821875142697849, -4.673326407553650697, 9.379999999999995453 ) ) ;
#5460 = CARTESIAN_POINT ( 'NONE',  ( 1.229367062500000385, -12.29022459553277002, -0.1770833340161300229 ) ) ;
#5461 = CARTESIAN_POINT ( 'NONE',  ( 0.8124729078102063129, -5.726445515403652209, 11.18394828327797441 ) ) ;
#5462 = ADVANCED_FACE ( 'NONE', ( #4883 ), #2506, .T. ) ;
#5463 = DIRECTION ( 'NONE',  ( -1.000000000000000000, -0.000000000000000000, 0.000000000000000000 ) ) ;
#5464 = ORIENTED_EDGE ( 'NONE', *, *, #8079, .F. ) ;
#5465 = CIRCLE ( 'NONE', #238, 3.000000000000000444 ) ;
#5466 = CARTESIAN_POINT ( 'NONE',  ( 1.499999999999999778, -13.86602540378444637, -2.104166668032260379 ) ) ;
#5467 = DIRECTION ( 'NONE',  ( -1.000000000000000000, -0.000000000000000000, -0.000000000000000000 ) ) ;
#5468 = PLANE ( 'NONE',  #5596 ) ;
#5469 = CARTESIAN_POINT ( 'NONE',  ( 25.00000000000000000, -4.000000000000000000, -10.00000000000000000 ) ) ;
#5470 = CARTESIAN_POINT ( 'NONE',  ( -1.500000000000002220, -13.86602540378444282, -1.708333333333333481 ) ) ;
#5471 = VERTEX_POINT ( 'NONE', #6308 ) ;
#5472 = FILL_AREA_STYLE_COLOUR ( '', #1172 ) ;
#5473 = DIRECTION ( 'NONE',  ( -1.000000000000000000, -0.000000000000000000, -0.000000000000000000 ) ) ;
#5474 = CARTESIAN_POINT ( 'NONE',  ( 3.345732310141667387, -3.345732310141653620, 11.90000000000000036 ) ) ;
#5475 = UNCERTAINTY_MEASURE_WITH_UNIT (LENGTH_MEASURE( 1.000000000000000082E-05 ), #4421, 'distance_accuracy_value', 'NONE');
#5476 = CARTESIAN_POINT ( 'NONE',  ( -3.181725716174720498E-16, -14.73205080756888385, -2.125000000000000000 ) ) ;
#5477 = EDGE_LOOP ( 'NONE', ( #4051, #650, #5371, #989 ) ) ;
#5478 = ORIENTED_EDGE ( 'NONE', *, *, #4996, .T. ) ;
#5479 = EDGE_CURVE ( 'NONE', #2644, #897, #7223, .T. ) ;
#5480 = AXIS2_PLACEMENT_3D ( 'NONE', #10140, #2920, #9388 ) ;
#5481 = CARTESIAN_POINT ( 'NONE',  ( 1.060575238724907038E-16, -11.26794919243112680, -0.8750000000000003331 ) ) ;
#5482 = ORIENTED_EDGE ( 'NONE', *, *, #9476, .F. ) ;
#5483 = CARTESIAN_POINT ( 'NONE',  ( 5.726445515403654873, -0.8124729078101852187, 9.816051716722022036 ) ) ;
#5484 = CARTESIAN_POINT ( 'NONE',  ( 4.432609873715410487, 7.613338054146847611, 0.000000000000000000 ) ) ;
#5485 = SURFACE_STYLE_FILL_AREA ( #6173 ) ;
#5486 = ORIENTED_EDGE ( 'NONE', *, *, #10406, .F. ) ;
#5487 = LINE ( 'NONE', #7934, #878 ) ;
#5488 = MECHANICAL_DESIGN_GEOMETRIC_PRESENTATION_REPRESENTATION (  '', ( #4637 ), #927 ) ;
#5489 = CARTESIAN_POINT ( 'NONE',  ( 4.430710083317573655, 0.7916369971161595354, 1.276051716722023333 ) ) ;
#5490 = EDGE_LOOP ( 'NONE', ( #5867, #3890 ) ) ;
#5491 = CIRCLE ( 'NONE', #3981, 1.500000000000000222 ) ;
#5492 = CARTESIAN_POINT ( 'NONE',  ( 1.500000000000000222, -13.00000000000000533, -1.562500001365593416 ) ) ;
#5493 = AXIS2_PLACEMENT_3D ( 'NONE', #7511, #3478, #5115 ) ;
#5494 = LINE ( 'NONE', #6342, #6592 ) ;
#5495 = ORIENTED_EDGE ( 'NONE', *, *, #7262, .F. ) ;
#5496 = DIRECTION ( 'NONE',  ( 1.000000000000000000, 0.000000000000000000, 0.000000000000000000 ) ) ;
#5497 = DIRECTION ( 'NONE',  ( 0.3420201433256627732, 0.9396926207859105373, -0.000000000000000000 ) ) ;
#5498 = CARTESIAN_POINT ( 'NONE',  ( -5.195105386651219348, -2.542276634908102295, 8.943948283277975975 ) ) ;
#5499 = EDGE_LOOP ( 'NONE', ( #1522, #3742, #8028, #2170 ) ) ;
#5500 = VECTOR ( 'NONE', #6447, 1000.000000000000000 ) ;
#5501 = CARTESIAN_POINT ( 'NONE',  ( 0.7499999999999991118, -14.29903810567666333, 0.3541666653010728805 ) ) ;
#5502 = EDGE_CURVE ( 'NONE', #6626, #4690, #3247, .T. ) ;
#5503 = CARTESIAN_POINT ( 'NONE',  ( 4.404961046766194599, -10.00000000000000000, -12.00000000000000000 ) ) ;
#5504 = ORIENTED_EDGE ( 'NONE', *, *, #2486, .F. ) ;
#5505 = CARTESIAN_POINT ( 'NONE',  ( -3.181725716174720991E-16, -14.73205080756888563, -0.6875000013655935271 ) ) ;
#5506 = AXIS2_PLACEMENT_3D ( 'NONE', #2864, #6088, #3608 ) ;
#5507 = FACE_OUTER_BOUND ( 'NONE', #10115, .T. ) ;
#5508 = FACE_OUTER_BOUND ( 'NONE', #5758, .T. ) ;
#5509 = DIRECTION ( 'NONE',  ( 0.000000000000000000, 0.000000000000000000, 1.000000000000000000 ) ) ;
#5510 = AXIS2_PLACEMENT_3D ( 'NONE', #5197, #5146, #9185 ) ;
#5511 = CARTESIAN_POINT ( 'NONE',  ( 10.71950000000001424, 0.000000000000000000, 0.000000000000000000 ) ) ;
#5512 = CARTESIAN_POINT ( 'NONE',  ( 2.148092372876330369, 4.215868657802593233, 11.05999999999999872 ) ) ;
#5513 = EDGE_CURVE ( 'NONE', #2194, #8250, #1088, .T. ) ;
#5514 = ADVANCED_FACE ( 'NONE', ( #3810 ), #3605, .T. ) ;
#5515 = CARTESIAN_POINT ( 'NONE',  ( 0.6146835312499993043, -14.06466310670085562, -1.427083334016129967 ) ) ;
#5516 = CARTESIAN_POINT ( 'NONE',  ( -5.446173322633801384, -0.7727076532861678615, 11.88394828327797548 ) ) ;
#5517 = PLANE ( 'NONE',  #4116 ) ;
#5518 = AXIS2_PLACEMENT_3D ( 'NONE', #8119, #6461, #3393 ) ;
#5519 = VERTEX_POINT ( 'NONE', #6193 ) ;
#5520 = APPLICATION_PROTOCOL_DEFINITION ( 'draft international standard', 'automotive_design', 1998, #6135 ) ;
#5521 = DIRECTION ( 'NONE',  ( -1.000000000000000000, 0.000000000000000000, -0.000000000000000000 ) ) ;
#5522 = DIRECTION ( 'NONE',  ( 0.000000000000000000, -0.000000000000000000, -1.000000000000000000 ) ) ;
#5523 = ORIENTED_EDGE ( 'NONE', *, *, #5311, .F. ) ;
#5524 = CARTESIAN_POINT ( 'NONE',  ( 25.00000000000000000, -4.000000000000000000, -12.00000000000000000 ) ) ;
#5525 = PLANE ( 'NONE',  #6612 ) ;
#5526 = VERTEX_POINT ( 'NONE', #5301 ) ;
#5527 = EDGE_CURVE ( 'NONE', #1984, #2738, #6888, .T. ) ;
#5528 =( NAMED_UNIT ( * ) PLANE_ANGLE_UNIT ( ) SI_UNIT ( $, .RADIAN. ) );
#5529 = DIRECTION ( 'NONE',  ( 0.000000000000000000, 0.000000000000000000, 1.000000000000000000 ) ) ;
#5530 = CARTESIAN_POINT ( 'NONE',  ( -3.345732310141667831, 3.345732310141653620, 7.699999999999998401 ) ) ;
#5531 = CARTESIAN_POINT ( 'NONE',  ( 1.500000000000000444, -12.13397459621556607, -0.9583333333333337034 ) ) ;
#5532 = VERTEX_POINT ( 'NONE', #5398 ) ;
#5533 = EDGE_LOOP ( 'NONE', ( #8408, #5567, #10084, #3154 ) ) ;
#5534 = CARTESIAN_POINT ( 'NONE',  ( -0.7499999999999997780, -11.70096189432334555, -0.8333333333333334814 ) ) ;
#5535 = ORIENTED_EDGE ( 'NONE', *, *, #215, .T. ) ;
#5536 = CARTESIAN_POINT ( 'NONE',  ( -4.687928535947287756, 0.6479879772514611780, 5.616051716722022746 ) ) ;
#5537 = CARTESIAN_POINT ( 'NONE',  ( -31.74999999999995737, 0.000000000000000000, 2.750000000000000000 ) ) ;
#5538 = LINE ( 'NONE', #9428, #9131 ) ;
#5539 = VERTEX_POINT ( 'NONE', #7042 ) ;
#5540 = DIRECTION ( 'NONE',  ( -1.000000000000000000, -0.000000000000000000, -0.000000000000000000 ) ) ;
#5541 = CARTESIAN_POINT ( 'NONE',  ( -5.110351332421769754, -2.708615832122969191, 13.73605171672202019 ) ) ;
#5542 = ORIENTED_EDGE ( 'NONE', *, *, #705, .T. ) ;
#5543 =( NAMED_UNIT ( * ) SI_UNIT ( $, .STERADIAN. ) SOLID_ANGLE_UNIT ( ) );
#5544 = ORIENTED_EDGE ( 'NONE', *, *, #1069, .F. ) ;
#5545 = DIRECTION ( 'NONE',  ( 0.000000000000000000, 0.000000000000000000, 1.000000000000000000 ) ) ;
#5546 = DIRECTION ( 'NONE',  ( -1.156482317317871478E-16, 1.000000000000000000, 0.000000000000000000 ) ) ;
#5547 = ORIENTED_EDGE ( 'NONE', *, *, #3766, .F. ) ;
#5548 = DIRECTION ( 'NONE',  ( -1.000000000000000000, -0.000000000000000000, -0.000000000000000000 ) ) ;
#5549 = LINE ( 'NONE', #3968, #4444 ) ;
#5550 = CARTESIAN_POINT ( 'NONE',  ( -0.8124729078102072011, 5.726445515403652209, 4.183948283277976188 ) ) ;
#5551 = EDGE_LOOP ( 'NONE', ( #10074, #842, #95, #4383 ) ) ;
#5552 = CARTESIAN_POINT ( 'NONE',  ( -2.607672531582950546E-16, -14.41955080893447416, -2.343750000682796930 ) ) ;
#5553 = ADVANCED_FACE ( 'NONE', ( #8641 ), #6139, .T. ) ;
#5554 = CARTESIAN_POINT ( 'NONE',  ( 2.500000000000007550, -31.99999999999999289, 0.000000000000000000 ) ) ;
#5555 = VERTEX_POINT ( 'NONE', #7697 ) ;
#5556 = LINE ( 'NONE', #9715, #3632 ) ;
#5557 = EDGE_CURVE ( 'NONE', #7636, #9635, #7248, .T. ) ;
#5558 = CARTESIAN_POINT ( 'NONE',  ( 12.99999999999999645, 19.99999999999999645, 9.000000000000000000 ) ) ;
#5559 = LINE ( 'NONE', #8803, #8131 ) ;
#5560 = DIRECTION ( 'NONE',  ( 0.000000000000000000, -1.000000000000000000, 1.026972870230479989E-15 ) ) ;
#5561 = CARTESIAN_POINT ( 'NONE',  ( 10.00000000000000000, 6.704570150427012543, -2.172265885002586661 ) ) ;
#5562 = CARTESIAN_POINT ( 'NONE',  ( -4.009529358847660596, 2.042957248827953265, 7.559999999999998721 ) ) ;
#5563 = AXIS2_PLACEMENT_3D ( 'NONE', #3107, #2855, #6077 ) ;
#5564 = CARTESIAN_POINT ( 'NONE',  ( 1.878224253233806040, 6.000000000000000000, -12.00000000000000000 ) ) ;
#5565 = CARTESIAN_POINT ( 'NONE',  ( -4.023224611898323033, 4.155232146225737111, 6.703948283277976650 ) ) ;
#5566 = PLANE ( 'NONE',  #5125 ) ;
#5567 = ORIENTED_EDGE ( 'NONE', *, *, #9331, .F. ) ;
#5568 = APPLICATION_PROTOCOL_DEFINITION ( 'draft international standard', 'automotive_design', 1998, #527 ) ;
#5569 = CARTESIAN_POINT ( 'NONE',  ( -4.900535883036028828, 2.496947748567499126, 1.959999999999999964 ) ) ;
#5570 = FACE_OUTER_BOUND ( 'NONE', #8478, .T. ) ;
#5571 = ORIENTED_EDGE ( 'NONE', *, *, #6696, .F. ) ;
#5572 = VECTOR ( 'NONE', #473, 1000.000000000000000 ) ;
#5573 = FACE_OUTER_BOUND ( 'NONE', #8154, .T. ) ;
#5574 = DIRECTION ( 'NONE',  ( 1.000000000000000000, 0.000000000000000000, 0.000000000000000000 ) ) ;
#5575 = DIRECTION ( 'NONE',  ( 0.000000000000000000, 0.000000000000000000, -1.000000000000000000 ) ) ;
#5576 = DIRECTION ( 'NONE',  ( 0.000000000000000000, 0.000000000000000000, 1.000000000000000000 ) ) ;
#5577 = CARTESIAN_POINT ( 'NONE',  ( 1.868979409283444415, 6.025400000000000311, -12.00000000000000000 ) ) ;
#5578 = CARTESIAN_POINT ( 'NONE',  ( 2.042957248827968808, -4.009529358847652603, 12.03999999999999915 ) ) ;
#5579 = STYLED_ITEM ( 'NONE', ( #5794 ), #4489 ) ;
#5580 = CARTESIAN_POINT ( 'NONE',  ( 0.7499999999999991118, -14.29903810567666333, -1.583333333333333481 ) ) ;
#5581 = ORIENTED_EDGE ( 'NONE', *, *, #10232, .T. ) ;
#5582 = EDGE_CURVE ( 'NONE', #7195, #6101, #1277, .T. ) ;
#5583 = EDGE_CURVE ( 'NONE', #2046, #10267, #10428, .T. ) ;
#5584 = ORIENTED_EDGE ( 'NONE', *, *, #1348, .F. ) ;
#5585 = CARTESIAN_POINT ( 'NONE',  ( 1.500000000000000222, -13.00000000000000533, -1.000000000000000000 ) ) ;
#5586 = AXIS2_PLACEMENT_3D ( 'NONE', #4630, #7124, #661 ) ;
#5587 = SURFACE_SIDE_STYLE ('',( #3052 ) ) ;
#5588 = EDGE_LOOP ( 'NONE', ( #5608, #4334, #4846, #5365 ) ) ;
#5589 = VECTOR ( 'NONE', #29, 1000.000000000000000 ) ;
#5590 = CARTESIAN_POINT ( 'NONE',  ( 0.000000000000000000, 0.000000000000000000, 3.000000000000000000 ) ) ;
#5591 = VECTOR ( 'NONE', #3019, 1000.000000000000000 ) ;
#5592 = DIRECTION ( 'NONE',  ( -0.000000000000000000, -0.000000000000000000, 1.000000000000000000 ) ) ;
#5593 = ORIENTED_EDGE ( 'NONE', *, *, #6848, .T. ) ;
#5594 = CARTESIAN_POINT ( 'NONE',  ( 1.999999999999975797, 15.00000000000000355, -6.000000000000009770 ) ) ;
#5595 = CARTESIAN_POINT ( 'NONE',  ( 3.119207202478379681, 3.244753828200549695, 0.9960517167220231949 ) ) ;
#5596 = AXIS2_PLACEMENT_3D ( 'NONE', #6955, #493, #10207 ) ;
#5597 = ORIENTED_EDGE ( 'NONE', *, *, #4802, .F. ) ;
#5598 = EDGE_CURVE ( 'NONE', #8600, #8355, #9023, .T. ) ;
#5599 = APPLICATION_CONTEXT ( 'automotive_design' ) ;
#5600 = ORIENTED_EDGE ( 'NONE', *, *, #1579, .F. ) ;
#5601 = AXIS2_PLACEMENT_3D ( 'NONE', #1237, #2089, #5362 ) ;
#5602 = CARTESIAN_POINT ( 'NONE',  ( 20.11292429676619520, -10.00000000000000000, -12.00000000000000000 ) ) ;
#5603 = CARTESIAN_POINT ( 'NONE',  ( 1.060575238724907038E-16, -11.26794919243112680, -1.875000000000000222 ) ) ;
#5604 = ORIENTED_EDGE ( 'NONE', *, *, #7737, .F. ) ;
#5605 = CARTESIAN_POINT ( 'NONE',  ( -2.496947748567517333, 4.900535883036019058, 7.839999999999999858 ) ) ;
#5606 = CARTESIAN_POINT ( 'NONE',  ( -2.000000000000000000, 0.000000000000000000, 0.000000000000000000 ) ) ;
#5607 = CARTESIAN_POINT ( 'NONE',  ( 5.711843387010018702, -0.9046671180729751738, 3.219999999999999751 ) ) ;
#5608 = ORIENTED_EDGE ( 'NONE', *, *, #4911, .T. ) ;
#5609 = CARTESIAN_POINT ( 'NONE',  ( -0.7500000000000007772, -14.29903810567666156, -0.2291666680322604066 ) ) ;
#5610 = DIRECTION ( 'NONE',  ( 0.000000000000000000, 0.000000000000000000, 1.000000000000000000 ) ) ;
#5611 = ORIENTED_EDGE ( 'NONE', *, *, #6737, .T. ) ;
#5612 = CARTESIAN_POINT ( 'NONE',  ( 0.000000000000000000, -10.00000000000000000, -12.00000000000000000 ) ) ;
#5613 = CARTESIAN_POINT ( 'NONE',  ( 12.12193523033274545, -7.750000000000000000, 0.000000000000000000 ) ) ;
#5614 = CYLINDRICAL_SURFACE ( 'NONE', #5243, 2.000000000000000000 ) ;
#5615 = DIRECTION ( 'NONE',  ( 0.9396926207859105373, 0.3420201433256627732, 0.000000000000000000 ) ) ;
#5616 = CARTESIAN_POINT ( 'NONE',  ( 4.000000000000000888, 8.357095590591340439, 1.552080310331536372 ) ) ;
#5617 = CARTESIAN_POINT ( 'NONE',  ( 2.148092372876330369, 4.215868657802593233, 5.459999999999997300 ) ) ;
#5618 = VERTEX_POINT ( 'NONE', #1224 ) ;
#5619 = CARTESIAN_POINT ( 'NONE',  ( 0.6146835312500001924, -11.93533689329915326, -0.2604166673494633377 ) ) ;
#5620 = CARTESIAN_POINT ( 'NONE',  ( 4.089228379062037178, -4.089228379062022967, 6.299999999999999822 ) ) ;
#5621 = DIRECTION ( 'NONE',  ( 0.3420201433256627732, -0.9396926207859105373, 0.000000000000000000 ) ) ;
#5622 = ITEM_DEFINED_TRANSFORMATION ( 'NONE', 'NONE', #8388,  #2101 ) ;
#5623 = CARTESIAN_POINT ( 'NONE',  ( -3.889087296526005044, -3.889087296526019255, 1.399999999999999689 ) ) ;
#5624 = LINE ( 'NONE', #2460, #9767 ) ;
#5625 = VERTEX_POINT ( 'NONE', #4448 ) ;
#5626 = CARTESIAN_POINT ( 'NONE',  ( -13.00000000000000000, 19.99999999999999645, -5.999999999999999112 ) ) ;
#5627 = CARTESIAN_POINT ( 'NONE',  ( 3.586028019667255595, -7.750000000000000000, 0.000000000000000000 ) ) ;
#5628 = CYLINDRICAL_SURFACE ( 'NONE', #9827, 3.000000000000000000 ) ;
#5629 = DIRECTION ( 'NONE',  ( 0.000000000000000000, 0.000000000000000000, 1.000000000000000000 ) ) ;
#5630 = LINE ( 'NONE', #7335, #4913 ) ;
#5631 = EDGE_CURVE ( 'NONE', #5003, #2005, #433, .T. ) ;
#5632 = CARTESIAN_POINT ( 'NONE',  ( -4.258245684917310925, -2.064922774268914019, 0.5439482832779766186 ) ) ;
#5633 = AXIS2_PLACEMENT_3D ( 'NONE', #9124, #3603, #5246 ) ;
#5634 = CARTESIAN_POINT ( 'NONE',  ( -0.7500000000000007772, -14.29903810567666156, -0.1666666666666669627 ) ) ;
#5635 = ORIENTED_EDGE ( 'NONE', *, *, #9432, .T. ) ;
#5636 = VERTEX_POINT ( 'NONE', #4502 ) ;
#5637 = DIRECTION ( 'NONE',  ( -1.000000000000000000, 0.000000000000000000, -0.000000000000000000 ) ) ;
#5638 = AXIS2_PLACEMENT_3D ( 'NONE', #8919, #8234, #4092 ) ;
#5639 = DIRECTION ( 'NONE',  ( -1.156482317317871478E-16, 1.000000000000000000, 0.000000000000000000 ) ) ;
#5640 = ORIENTED_EDGE ( 'NONE', *, *, #7781, .F. ) ;
#5641 = CARTESIAN_POINT ( 'NONE',  ( -3.345732310141667831, 3.345732310141653620, 2.099999999999999645 ) ) ;
#5642 = EDGE_CURVE ( 'NONE', #4597, #789, #7747, .T. ) ;
#5643 = VERTEX_POINT ( 'NONE', #6936 ) ;
#5644 = ADVANCED_FACE ( 'NONE', ( #9607 ), #9918, .F. ) ;
#5645 = EDGE_CURVE ( 'NONE', #3690, #2579, #3923, .T. ) ;
#5646 = CARTESIAN_POINT ( 'NONE',  ( 4.173491630687861331, 2.231261971483781359, 3.936051716722023031 ) ) ;
#5647 = ORIENTED_EDGE ( 'NONE', *, *, #796, .F. ) ;
#5648 =( GEOMETRIC_REPRESENTATION_CONTEXT ( 3 ) GLOBAL_UNCERTAINTY_ASSIGNED_CONTEXT ( ( #1209 ) ) GLOBAL_UNIT_ASSIGNED_CONTEXT ( ( #6662, #9010, #5862 ) ) REPRESENTATION_CONTEXT ( 'NONE', 'WORKASPACE' ) );
#5649 =( LENGTH_UNIT ( ) NAMED_UNIT ( * ) SI_UNIT ( .MILLI., .METRE. ) );
#5650 = ORIENTED_EDGE ( 'NONE', *, *, #6334, .F. ) ;
#5651 = CARTESIAN_POINT ( 'NONE',  ( -2.000000000000000000, 52.93638525830372998, 8.843061888689529582 ) ) ;
#5652 = LINE ( 'NONE', #2323, #173 ) ;
#5653 = EDGE_LOOP ( 'NONE', ( #9043, #1474, #724, #880 ) ) ;
#5654 = CARTESIAN_POINT ( 'NONE',  ( 4.900535883036028828, -2.496947748567499126, 3.359999999999999876 ) ) ;
#5655 = DIRECTION ( 'NONE',  ( -0.3420201433256627732, -0.9396926207859105373, 0.000000000000000000 ) ) ;
#5656 = CARTESIAN_POINT ( 'NONE',  ( 0.9480714621563713917, 5.418398423912717199, 12.72394828327797711 ) ) ;
#5657 = EDGE_LOOP ( 'NONE', ( #3719, #3668, #3524, #1416 ) ) ;
#5658 = ADVANCED_FACE ( 'NONE', ( #4705 ), #3863, .T. ) ;
#5659 = CARTESIAN_POINT ( 'NONE',  ( -1.500000000000000000, -12.13397459621556607, 0.1458333319677399265 ) ) ;
#5660 = ORIENTED_EDGE ( 'NONE', *, *, #8829, .F. ) ;
#5661 = DIRECTION ( 'NONE',  ( 0.000000000000000000, 0.000000000000000000, -1.000000000000000000 ) ) ;
#5662 = CARTESIAN_POINT ( 'NONE',  ( 4.000000000000000888, 6.745408891279613961, -5.171987904998036178 ) ) ;
#5663 = CARTESIAN_POINT ( 'NONE',  ( 1.300000000000000044, -1.478016689125442706, 1.843143693225357538E-15 ) ) ;
#5664 = DIRECTION ( 'NONE',  ( 0.000000000000000000, 0.000000000000000000, 1.000000000000000000 ) ) ;
#5665 = CARTESIAN_POINT ( 'NONE',  ( 3.279728542977952799, -3.411736077305369541, 2.503948283277976472 ) ) ;
#5666 = EDGE_LOOP ( 'NONE', ( #2787, #9076, #8420, #7825 ) ) ;
#5667 = LINE ( 'NONE', #1707, #4755 ) ;
#5668 = CARTESIAN_POINT ( 'NONE',  ( -0.9046671180729963790, 5.711843387010016926, 7.979999999999999538 ) ) ;
#5669 = PRODUCT_RELATED_PRODUCT_CATEGORY ( 'part', '', ( #5453 ) ) ;
#5670 = CARTESIAN_POINT ( 'NONE',  ( 1.878224253233805818, -10.00000000000000000, -12.00000000000000000 ) ) ;
#5671 = VECTOR ( 'NONE', #6604, 1000.000000000000000 ) ;
#5672 = SHAPE_DEFINITION_REPRESENTATION ( #8765, #8347 ) ;
#5673 = CARTESIAN_POINT ( 'NONE',  ( 5.432285873273257515, 0.8603895577212793411, 3.079999999999999627 ) ) ;
#5674 = AXIS2_PLACEMENT_3D ( 'NONE', #3662, #383, #10143 ) ;
#5675 = CARTESIAN_POINT ( 'NONE',  ( 3.000000000000000000, 0.000000000000000000, -1.600000000000000311 ) ) ;
#5676 = FACE_OUTER_BOUND ( 'NONE', #6494, .T. ) ;
#5677 = DIRECTION ( 'NONE',  ( -1.000000000000000000, 0.000000000000000000, 0.000000000000000000 ) ) ;
#5678 = CARTESIAN_POINT ( 'NONE',  ( 24.68830583033274806, 3.750000000000000000, -12.00000000000000000 ) ) ;
#5679 = AXIS2_PLACEMENT_3D ( 'NONE', #1560, #4722, #7381 ) ;
#5680 = DIRECTION ( 'NONE',  ( -0.3420201433256627732, 0.9396926207859105373, 0.000000000000000000 ) ) ;
#5681 = CARTESIAN_POINT ( 'NONE',  ( 1.500000000000000222, -13.00000000000000533, -2.500000000000000000 ) ) ;
#5682 = CARTESIAN_POINT ( 'NONE',  ( 4.258245684917310037, 2.064922774268912686, 4.743948283277974909 ) ) ;
#5683 = CARTESIAN_POINT ( 'NONE',  ( 0.7499999999999991118, -14.29903810567666333, -0.08333333333333370341 ) ) ;
#5684 = ORIENTED_EDGE ( 'NONE', *, *, #7077, .F. ) ;
#5685 = ORIENTED_EDGE ( 'NONE', *, *, #8455, .F. ) ;
#5686 = DIRECTION ( 'NONE',  ( -0.000000000000000000, -0.000000000000000000, 1.000000000000000000 ) ) ;
#5687 = EDGE_CURVE ( 'NONE', #8580, #8403, #4027, .T. ) ;
#5688 = FACE_OUTER_BOUND ( 'NONE', #4539, .T. ) ;
#5689 = ORIENTED_EDGE ( 'NONE', *, *, #9219, .F. ) ;
#5690 = CARTESIAN_POINT ( 'NONE',  ( -2.042957248827969252, 4.009529358847651714, 5.039999999999999147 ) ) ;
#5691 = DIRECTION ( 'NONE',  ( -0.000000000000000000, 0.000000000000000000, -1.000000000000000000 ) ) ;
#5692 = ORIENTED_EDGE ( 'NONE', *, *, #3272, .T. ) ;
#5693 = CARTESIAN_POINT ( 'NONE',  ( -2.064922774268895811, -4.258245684917318918, 10.65605171672202012 ) ) ;
#5694 = VERTEX_POINT ( 'NONE', #3180 ) ;
#5695 = EDGE_CURVE ( 'NONE', #4827, #1061, #6441, .T. ) ;
#5696 = DIRECTION ( 'NONE',  ( -1.000000000000000000, 0.000000000000000000, 0.000000000000000000 ) ) ;
#5697 = EDGE_CURVE ( 'NONE', #8159, #6209, #4820, .T. ) ;
#5698 =( LENGTH_UNIT ( ) NAMED_UNIT ( * ) SI_UNIT ( .MILLI., .METRE. ) );
#5699 = ORIENTED_EDGE ( 'NONE', *, *, #7412, .T. ) ;
#5700 = CARTESIAN_POINT ( 'NONE',  ( -4.900535883036028828, 2.496947748567499126, 1.959999999999999964 ) ) ;
#5701 = PLANE ( 'NONE',  #4980 ) ;
#5702 = CARTESIAN_POINT ( 'NONE',  ( 5.152728359536493663, 2.625446233515533745, 0.1399999999999999856 ) ) ;
#5703 = ORIENTED_EDGE ( 'NONE', *, *, #4535, .T. ) ;
#5704 = CARTESIAN_POINT ( 'NONE',  ( -1.500000000000000000, -12.13397459621556607, -0.3541666680322600458 ) ) ;
#5705 = SURFACE_SIDE_STYLE ('',( #8952 ) ) ;
#5706 = EDGE_LOOP ( 'NONE', ( #1313, #6414 ) ) ;
#5707 = PRODUCT_DEFINITION_SHAPE ( 'NONE', 'NONE',  #10503 ) ;
#5708 = EDGE_CURVE ( 'NONE', #729, #4172, #8067, .T. ) ;
#5709 = CARTESIAN_POINT ( 'NONE',  ( 20.12216914071655793, -10.02539999999999942, -12.00000000000000000 ) ) ;
#5710 = PLANE ( 'NONE',  #4576 ) ;
#5711 = DIRECTION ( 'NONE',  ( -1.000000000000000000, -0.000000000000000000, -0.000000000000000000 ) ) ;
#5712 = CYLINDRICAL_SURFACE ( 'NONE', #6746, 1.599999999999992983 ) ;
#5713 = FACE_OUTER_BOUND ( 'NONE', #7414, .T. ) ;
#5714 = CARTESIAN_POINT ( 'NONE',  ( -4.258245684917310925, -2.064922774268914019, 3.343948283277975886 ) ) ;
#5715 = ORIENTED_EDGE ( 'NONE', *, *, #2265, .T. ) ;
#5716 = DIRECTION ( 'NONE',  ( 0.000000000000000000, -0.000000000000000000, -1.000000000000000000 ) ) ;
#5717 = CARTESIAN_POINT ( 'NONE',  ( 0.9046671180729951578, -5.711843387010016926, 0.9799999999999997602 ) ) ;
#5718 = CARTESIAN_POINT ( 'NONE',  ( 0.000000000000000000, -0.7390083445627200209, 1.280000000000001137 ) ) ;
#5719 = ADVANCED_FACE ( 'NONE', ( #57 ), #3232, .F. ) ;
#5720 = CARTESIAN_POINT ( 'NONE',  ( 8.000000000000001776, 6.704570150427012543, -2.172265885002586661 ) ) ;
#5721 = CARTESIAN_POINT ( 'NONE',  ( 12.99999999999999645, 19.99999999999999645, 6.000000000000000000 ) ) ;
#5722 = DIRECTION ( 'NONE',  ( 1.000000000000000000, 0.000000000000000000, 0.000000000000000000 ) ) ;
#5723 = VECTOR ( 'NONE', #7214, 1000.000000000000000 ) ;
#5724 = DIRECTION ( 'NONE',  ( 0.000000000000000000, 0.000000000000000000, 1.000000000000000000 ) ) ;
#5725 = FACE_OUTER_BOUND ( 'NONE', #6587, .T. ) ;
#5726 = CARTESIAN_POINT ( 'NONE',  ( -0.6162731882459178134, -4.458484982038665834, 4.916051716722023457 ) ) ;
#5727 = LINE ( 'NONE', #7279, #3036 ) ;
#5728 = CARTESIAN_POINT ( 'NONE',  ( 3.969226411068985882, -2.122056237541205981, 7.963948283277976437 ) ) ;
#5729 = DIRECTION ( 'NONE',  ( -1.000000000000000000, 0.000000000000000000, 0.000000000000000000 ) ) ;
#5730 = CIRCLE ( 'NONE', #8152, 2.000000000000000000 ) ;
#5731 = VERTEX_POINT ( 'NONE', #1485 ) ;
#5732 = ADVANCED_FACE ( 'NONE', ( #3977 ), #9500, .T. ) ;
#5733 = VECTOR ( 'NONE', #905, 1000.000000000000000 ) ;
#5734 = ORIENTED_EDGE ( 'NONE', *, *, #8760, .T. ) ;
#5735 = LINE ( 'NONE', #87, #2736 ) ;
#5736 = VECTOR ( 'NONE', #1664, 1000.000000000000000 ) ;
#5737 = DIRECTION ( 'NONE',  ( 0.000000000000000000, 0.000000000000000000, 1.000000000000000000 ) ) ;
#5738 = EDGE_CURVE ( 'NONE', #1584, #10233, #799, .T. ) ;
#5739 = VERTEX_POINT ( 'NONE', #3128 ) ;
#5740 = VECTOR ( 'NONE', #4436, 1000.000000000000000 ) ;
#5741 = CARTESIAN_POINT ( 'NONE',  ( -4.215868657802586128, -2.148092372876348133, 4.339999999999999858 ) ) ;
#5742 = SURFACE_STYLE_FILL_AREA ( #10323 ) ;
#5743 = ORIENTED_EDGE ( 'NONE', *, *, #7899, .F. ) ;
#5744 = VECTOR ( 'NONE', #9478, 1000.000000000000000 ) ;
#5745 = CARTESIAN_POINT ( 'NONE',  ( -0.8323763977770610722, 4.658724279160015413, 11.77605171672202289 ) ) ;
#5746 = LINE ( 'NONE', #7202, #8528 ) ;
#5747 = ADVANCED_FACE ( 'NONE', ( #5454 ), #1429, .T. ) ;
#5748 = ORIENTED_EDGE ( 'NONE', *, *, #9343, .T. ) ;
#5749 = VERTEX_POINT ( 'NONE', #7093 ) ;
#5750 = CARTESIAN_POINT ( 'NONE',  ( 0.000000000000000000, -4.000000000000000000, 0.000000000000000000 ) ) ;
#5751 =( GEOMETRIC_REPRESENTATION_CONTEXT ( 3 ) GLOBAL_UNCERTAINTY_ASSIGNED_CONTEXT ( ( #7677 ) ) GLOBAL_UNIT_ASSIGNED_CONTEXT ( ( #8562, #6904, #10158 ) ) REPRESENTATION_CONTEXT ( 'NONE', 'WORKASPACE' ) );
#5752 = PLANE ( 'NONE',  #9495 ) ;
#5753 = ORIENTED_EDGE ( 'NONE', *, *, #7107, .F. ) ;
#5754 =( BOUNDED_CURVE ( )  B_SPLINE_CURVE ( 2, ( #7860, #2244, #5361, #9405, #9515, #5466, #6205 ),
 .UNSPECIFIED., .F., .F. ) 
 B_SPLINE_CURVE_WITH_KNOTS ( ( 3, 2, 2, 3 ),
 ( 0.08333333333333325932, 0.1111111111111110494, 0.1388888888888888673, 0.1666666666666666574 ),
 .UNSPECIFIED. ) 
 CURVE ( )  GEOMETRIC_REPRESENTATION_ITEM ( )  RATIONAL_B_SPLINE_CURVE ( ( 1.000000000000000222, 0.8660254037844383745, 1.000000000000000000, 0.8660254037844387076, 1.000000000000000000, 0.8660254037844387076, 1.000000000000000000 ) ) 
 REPRESENTATION_ITEM ( '' )  );
#5755 = CARTESIAN_POINT ( 'NONE',  ( -2.496947748567517333, 4.900535883036019058, 5.039999999999999147 ) ) ;
#5756 = CARTESIAN_POINT ( 'NONE',  ( -3.889087296526005044, -3.889087296526019255, 6.999999999999999112 ) ) ;
#5757 = CARTESIAN_POINT ( 'NONE',  ( 3.951860609387084722, 3.826313983664940022, 10.20394828327797399 ) ) ;
#5758 = EDGE_LOOP ( 'NONE', ( #3692, #8102, #6558, #9293 ) ) ;
#5759 = VECTOR ( 'NONE', #10260, 1000.000000000000000 ) ;
#5760 = CARTESIAN_POINT ( 'NONE',  ( 1.229367062500000385, -12.29022459553277002, -0.6770833340161300784 ) ) ;
#5761 = VECTOR ( 'NONE', #9180, 1000.000000000000000 ) ;
#5762 = ORIENTED_EDGE ( 'NONE', *, *, #8502, .F. ) ;
#5763 = VECTOR ( 'NONE', #9070, 1000.000000000000000 ) ;
#5764 = DIRECTION ( 'NONE',  ( 0.000000000000000000, 0.000000000000000000, 1.000000000000000000 ) ) ;
#5765 = CARTESIAN_POINT ( 'NONE',  ( 5.999999999999999112, -27.00000000000000711, -17.00000000000000000 ) ) ;
#5766 = CARTESIAN_POINT ( 'NONE',  ( 7.401486830834375884E-15, -31.99999999999999289, 0.000000000000000000 ) ) ;
#5767 = DIRECTION ( 'NONE',  ( 0.3420201433256627732, -0.9396926207859105373, 0.000000000000000000 ) ) ;
#5768 = CARTESIAN_POINT ( 'NONE',  ( -1.229367062500000163, -12.29022459553277002, -1.635416667349463227 ) ) ;
#5769 = CARTESIAN_POINT ( 'NONE',  ( -4.258245684917310925, -2.064922774268914019, 0.5439482832779766186 ) ) ;
#5770 = ORIENTED_EDGE ( 'NONE', *, *, #9849, .T. ) ;
#5771 = CARTESIAN_POINT ( 'NONE',  ( -0.6146835312499998594, -11.93533689329915326, -0.1770833340161300506 ) ) ;
#5772 = EDGE_CURVE ( 'NONE', #371, #6398, #5556, .T. ) ;
#5773 = ADVANCED_FACE ( 'NONE', ( #8012 ), #9228, .F. ) ;
#5774 = CARTESIAN_POINT ( 'NONE',  ( 2.625446233515515537, 5.152728359536502545, 2.659999999999998366 ) ) ;
#5775 = DIRECTION ( 'NONE',  ( -1.000000000000000000, 0.000000000000000000, -0.000000000000000000 ) ) ;
#5776 = CARTESIAN_POINT ( 'NONE',  ( 5.152728359536493663, 2.625446233515533745, 11.33999999999999808 ) ) ;
#5777 = DIRECTION ( 'NONE',  ( 0.000000000000000000, -1.000000000000000000, 0.000000000000000000 ) ) ;
#5778 = DIRECTION ( 'NONE',  ( 0.000000000000000000, 0.000000000000000000, 1.000000000000000000 ) ) ;
#5779 = DIRECTION ( 'NONE',  ( 0.3420201433256627732, -0.9396926207859105373, 0.000000000000000000 ) ) ;
#5780 = DIRECTION ( 'NONE',  ( 0.000000000000000000, 0.000000000000000000, 1.000000000000000000 ) ) ;
#5781 = CARTESIAN_POINT ( 'NONE',  ( -4.430710083317573655, -0.7916369971161599794, 5.476051716722023066 ) ) ;
#5782 = LINE ( 'NONE', #6581, #1686 ) ;
#5783 = EDGE_CURVE ( 'NONE', #4315, #1597, #1598, .T. ) ;
#5784 = CARTESIAN_POINT ( 'NONE',  ( -4.258245684917310925, -2.064922774268914019, 8.943948283277975975 ) ) ;
#5785 = DIRECTION ( 'NONE',  ( 0.000000000000000000, 0.000000000000000000, 1.000000000000000000 ) ) ;
#5786 = ORIENTED_EDGE ( 'NONE', *, *, #10280, .T. ) ;
#5787 = CARTESIAN_POINT ( 'NONE',  ( -4.940838830814703542, 2.417848759854245078, 8.556051716722022249 ) ) ;
#5788 = EDGE_LOOP ( 'NONE', ( #3164, #8880, #9916, #8089 ) ) ;
#5789 = FACE_OUTER_BOUND ( 'NONE', #785, .T. ) ;
#5790 = CARTESIAN_POINT ( 'NONE',  ( 1.658513752677435171, -10.60364963909571401, 0.000000000000000000 ) ) ;
#5791 = ORIENTED_EDGE ( 'NONE', *, *, #7611, .T. ) ;
#5792 = CARTESIAN_POINT ( 'NONE',  ( -4.009529358847660596, 2.042957248827953265, 4.759999999999999787 ) ) ;
#5793 = AXIS2_PLACEMENT_3D ( 'NONE', #840, #3171, #8369 ) ;
#5794 = PRESENTATION_STYLE_ASSIGNMENT (( #8837 ) ) ;
#5795 = ORIENTED_EDGE ( 'NONE', *, *, #3227, .T. ) ;
#5796 = CARTESIAN_POINT ( 'NONE',  ( 3.411736077305382420, -3.279728542977940364, 10.09605171672202140 ) ) ;
#5797 = DIRECTION ( 'NONE',  ( 0.000000000000000000, 0.000000000000000000, 1.000000000000000000 ) ) ;
#5798 = ORIENTED_EDGE ( 'NONE', *, *, #3486, .T. ) ;
#5799 = SURFACE_STYLE_FILL_AREA ( #4214 ) ;
#5800 = ORIENTED_EDGE ( 'NONE', *, *, #2088, .F. ) ;
#5801 = CIRCLE ( 'NONE', #5302, 2.000000000000000000 ) ;
#5802 = DIRECTION ( 'NONE',  ( -1.000000000000000000, 0.000000000000000000, -0.000000000000000000 ) ) ;
#5803 = CARTESIAN_POINT ( 'NONE',  ( -1.499999999999999778, -12.13397459621556784, -0.2916666666666666852 ) ) ;
#5804 = ORIENTED_EDGE ( 'NONE', *, *, #6685, .F. ) ;
#5805 = CARTESIAN_POINT ( 'NONE',  ( -0.8603895577212598011, -5.432285873273260179, 3.919999999999999929 ) ) ;
#5806 = CARTESIAN_POINT ( 'NONE',  ( -2.625446233515515981, -5.152728359536500768, 4.059999999999999609 ) ) ;
#5807 = CARTESIAN_POINT ( 'NONE',  ( 3.889087296526005488, 3.889087296526018811, 2.799999999999999378 ) ) ;
#5808 = VERTEX_POINT ( 'NONE', #8907 ) ;
#5809 = CARTESIAN_POINT ( 'NONE',  ( 0.6146835312500001924, -11.93533689329915326, -1.135416667349463227 ) ) ;
#5810 = VECTOR ( 'NONE', #5451, 1000.000000000000000 ) ;
#5811 =( LENGTH_UNIT ( ) NAMED_UNIT ( * ) SI_UNIT ( .MILLI., .METRE. ) );
#5812 = ORIENTED_EDGE ( 'NONE', *, *, #4934, .F. ) ;
#5813 =( BOUNDED_CURVE ( )  B_SPLINE_CURVE ( 2, ( #1106, #9115, #4332, #3285, #6510, #517, #2009 ),
 .UNSPECIFIED., .F., .F. ) 
 B_SPLINE_CURVE_WITH_KNOTS ( ( 3, 2, 2, 3 ),
 ( 0.08333333333333339810, 0.1111111111111111466, 0.1388888888888889228, 0.1666666666666666574 ),
 .UNSPECIFIED. ) 
 CURVE ( )  GEOMETRIC_REPRESENTATION_ITEM ( )  RATIONAL_B_SPLINE_CURVE ( ( 0.9999999999999996669, 0.8660254037844390407, 1.000000000000000000, 0.8660254037844387076, 1.000000000000000000, 0.8660254037844387076, 1.000000000000000000 ) ) 
 REPRESENTATION_ITEM ( '' )  );
#5814 = FACE_OUTER_BOUND ( 'NONE', #10062, .T. ) ;
#5815 = CYLINDRICAL_SURFACE ( 'NONE', #1030, 1.500000000000000222 ) ;
#5816 = DIRECTION ( 'NONE',  ( -5.694029147589358720E-15, 0.000000000000000000, 1.000000000000000000 ) ) ;
#5817 = EDGE_LOOP ( 'NONE', ( #402, #7399, #10364, #4543 ) ) ;
#5818 = VECTOR ( 'NONE', #5343, 1000.000000000000000 ) ;
#5819 = LINE ( 'NONE', #5663, #7388 ) ;
#5820 = EDGE_CURVE ( 'NONE', #2302, #3003, #4872, .T. ) ;
#5821 = CARTESIAN_POINT ( 'NONE',  ( -0.6146835312500006365, -14.06466310670085562, -1.510416667349463227 ) ) ;
#5822 = CARTESIAN_POINT ( 'NONE',  ( 3.181980515339458471, 3.181980515339470461, 13.99999999999999822 ) ) ;
#5823 = ORIENTED_EDGE ( 'NONE', *, *, #10433, .F. ) ;
#5824 = DIRECTION ( 'NONE',  ( -0.000000000000000000, -0.000000000000000000, -1.000000000000000000 ) ) ;
#5825 = CARTESIAN_POINT ( 'NONE',  ( -2.496947748567517333, 4.900535883036019058, 2.239999999999999769 ) ) ;
#5826 = PRESENTATION_LAYER_ASSIGNMENT (  '', '', ( #4637 ) ) ;
#5827 = CARTESIAN_POINT ( 'NONE',  ( 10.00000000000000178, 0.000000000000000000, 0.000000000000000000 ) ) ;
#5828 = CARTESIAN_POINT ( 'NONE',  ( -5.711843387010019590, 0.9046671180729746187, 7.419999999999999041 ) ) ;
#5829 = DIRECTION ( 'NONE',  ( -1.000000000000000000, 0.000000000000000000, -0.000000000000000000 ) ) ;
#5830 = ADVANCED_FACE ( 'NONE', ( #4281 ), #6713, .T. ) ;
#5831 = PLANE ( 'NONE',  #108 ) ;
#5832 = ADVANCED_FACE ( 'NONE', ( #7476 ), #901, .F. ) ;
#5833 = DIRECTION ( 'NONE',  ( 0.000000000000000000, 0.000000000000000000, 1.000000000000000000 ) ) ;
#5834 = CARTESIAN_POINT ( 'NONE',  ( -2.064922774268895811, -4.258245684917318918, 2.256051716722022871 ) ) ;
#5835 = LINE ( 'NONE', #6790, #697 ) ;
#5836 = AXIS2_PLACEMENT_3D ( 'NONE', #6391, #9541, #3167 ) ;
#5837 = CARTESIAN_POINT ( 'NONE',  ( -4.258245684917310925, -2.064922774268914019, 3.343948283277975886 ) ) ;
#5838 = DIRECTION ( 'NONE',  ( 1.000000000000000000, 2.312964634635742957E-16, 0.000000000000000000 ) ) ;
#5839 = ORIENTED_EDGE ( 'NONE', *, *, #1197, .T. ) ;
#5840 = CARTESIAN_POINT ( 'NONE',  ( 2.542276634908080535, 5.195105386651229118, 3.656051716722022782 ) ) ;
#5841 = ADVANCED_FACE ( 'NONE', ( #3389 ), #2546, .T. ) ;
#5842 = CARTESIAN_POINT ( 'NONE',  ( 9.000000000000000000, 19.99999999999999645, 17.00000000000000000 ) ) ;
#5843 = CARTESIAN_POINT ( 'NONE',  ( 1.300000000000000044, 1.690103923579304181E-15, 1.280000000000000249 ) ) ;
#5844 = VERTEX_POINT ( 'NONE', #267 ) ;
#5845 = VECTOR ( 'NONE', #3518, 1000.000000000000000 ) ;
#5846 = CARTESIAN_POINT ( 'NONE',  ( 1.878224253233806040, -10.00000000000000000, -12.00000000000000000 ) ) ;
#5847 = DIRECTION ( 'NONE',  ( -1.000000000000000000, -0.000000000000000000, -0.000000000000000000 ) ) ;
#5848 = VERTEX_POINT ( 'NONE', #2695 ) ;
#5849 = CARTESIAN_POINT ( 'NONE',  ( 0.8323763977770604061, -4.658724279160015413, 4.776051716722021112 ) ) ;
#5850 = CARTESIAN_POINT ( 'NONE',  ( 5.999999999999999112, 26.99999999999999289, -17.00000000000000000 ) ) ;
#5851 = ORIENTED_EDGE ( 'NONE', *, *, #2618, .F. ) ;
#5852 = DIRECTION ( 'NONE',  ( 0.000000000000000000, 1.000000000000000000, 0.000000000000000000 ) ) ;
#5853 = VERTEX_POINT ( 'NONE', #2649 ) ;
#5854 = DIRECTION ( 'NONE',  ( 1.000000000000000000, 0.000000000000000000, 0.000000000000000000 ) ) ;
#5855 = PRESENTATION_STYLE_ASSIGNMENT (( #4118 ) ) ;
#5856 = EDGE_LOOP ( 'NONE', ( #9307, #5232, #2743, #52 ) ) ;
#5857 = CARTESIAN_POINT ( 'NONE',  ( -3.889087296526005044, -3.889087296526019255, 9.799999999999998934 ) ) ;
#5858 = CARTESIAN_POINT ( 'NONE',  ( -4.900535883036028828, 2.496947748567499126, 7.559999999999998721 ) ) ;
#5859 = CARTESIAN_POINT ( 'NONE',  ( 4.900535883036028828, -2.496947748567499126, 11.75999999999999979 ) ) ;
#5860 = VERTEX_POINT ( 'NONE', #5078 ) ;
#5861 = CARTESIAN_POINT ( 'NONE',  ( -0.6146835312499998594, -11.93533689329915326, -0.05208333401612993963 ) ) ;
#5862 =( NAMED_UNIT ( * ) SI_UNIT ( $, .STERADIAN. ) SOLID_ANGLE_UNIT ( ) );
#5863 = VERTEX_POINT ( 'NONE', #2495 ) ;
#5864 = DIRECTION ( 'NONE',  ( -1.000000000000000000, -0.000000000000000000, -0.000000000000000000 ) ) ;
#5865 = DIRECTION ( 'NONE',  ( -0.8660254037844402619, 0.000000000000000000, -0.4999999999999972244 ) ) ;
#5866 = CARTESIAN_POINT ( 'NONE',  ( 1.500000000000000222, -12.13397459621556784, -1.020833334698926897 ) ) ;
#5867 = ORIENTED_EDGE ( 'NONE', *, *, #6749, .F. ) ;
#5868 = DIRECTION ( 'NONE',  ( -1.000000000000000000, -0.000000000000000000, -0.000000000000000000 ) ) ;
#5869 = CARTESIAN_POINT ( 'NONE',  ( -1.229367062500000163, -13.70977540446723708, -1.552083334016130189 ) ) ;
#5870 = EDGE_CURVE ( 'NONE', #8379, #7188, #5987, .T. ) ;
#5871 = CARTESIAN_POINT ( 'NONE',  ( -4.673326407553653361, 0.7401821875142517992, 13.01999999999999424 ) ) ;
#5872 = EDGE_LOOP ( 'NONE', ( #4561, #1825, #5436, #6450 ) ) ;
#5873 = CARTESIAN_POINT ( 'NONE',  ( 0.000000000000000000, 0.000000000000000000, 6.999999999999999112 ) ) ;
#5874 = DIRECTION ( 'NONE',  ( -0.9396926207859105373, 0.3420201433256627732, 0.000000000000000000 ) ) ;
#5875 = CARTESIAN_POINT ( 'NONE',  ( 10.00000000000000000, 0.000000000000000000, 0.000000000000000000 ) ) ;
#5876 = EDGE_CURVE ( 'NONE', #10421, #1372, #9766, .T. ) ;
#5877 = CARTESIAN_POINT ( 'NONE',  ( -0.8603895577212598011, -5.432285873273260179, 3.919999999999999929 ) ) ;
#5878 = DIRECTION ( 'NONE',  ( 0.000000000000000000, 0.000000000000000000, 1.000000000000000000 ) ) ;
#5879 = DIRECTION ( 'NONE',  ( 0.000000000000000000, -1.000000000000000000, 0.000000000000000000 ) ) ;
#5880 = LINE ( 'NONE', #6034, #10471 ) ;
#5881 = CARTESIAN_POINT ( 'NONE',  ( -4.430710083317573655, -0.7916369971161599794, 2.676051716722023244 ) ) ;
#5882 = CARTESIAN_POINT ( 'NONE',  ( 0.6146835312499993043, -14.06466310670085562, -1.802083334016129745 ) ) ;
#5883 = CARTESIAN_POINT ( 'NONE',  ( 4.458484982038663169, 0.6162731882459350219, 4.883948283277976365 ) ) ;
#5884 = CARTESIAN_POINT ( 'NONE',  ( -5.999999999999999112, -27.00000000000000711, -14.00000000000000178 ) ) ;
#5885 = ORIENTED_EDGE ( 'NONE', *, *, #7389, .F. ) ;
#5886 = EDGE_CURVE ( 'NONE', #8274, #10315, #1748, .T. ) ;
#5887 = CARTESIAN_POINT ( 'NONE',  ( -5.418398423912711870, -0.9480714621563917088, 5.476051716722023066 ) ) ;
#5888 = CARTESIAN_POINT ( 'NONE',  ( 1.300000000000000044, 0.000000000000000000, 0.000000000000000000 ) ) ;
#5889 = FACE_OUTER_BOUND ( 'NONE', #1136, .T. ) ;
#5890 = VERTEX_POINT ( 'NONE', #8956 ) ;
#5891 = CARTESIAN_POINT ( 'NONE',  ( 2.148092372876330369, 4.215868657802594122, 13.85999999999999943 ) ) ;
#5892 = CARTESIAN_POINT ( 'NONE',  ( 10.00000000000000000, 0.000000000000000000, 0.000000000000000000 ) ) ;
#5893 = CIRCLE ( 'NONE', #835, 1.219500000000000028 ) ;
#5894 = CARTESIAN_POINT ( 'NONE',  ( 2.064922774268895811, 4.258245684917319807, 12.05605171672202047 ) ) ;
#5895 = EDGE_CURVE ( 'NONE', #4888, #1146, #7523, .T. ) ;
#5896 = PRESENTATION_LAYER_ASSIGNMENT (  '', '', ( #7777 ) ) ;
#5897 = CARTESIAN_POINT ( 'NONE',  ( -2.399999999999999911, 0.000000000000000000, -14.00000000000000178 ) ) ;
#5898 = EDGE_CURVE ( 'NONE', #8600, #9521, #5491, .T. ) ;
#5899 = ORIENTED_EDGE ( 'NONE', *, *, #2416, .T. ) ;
#5900 = DIRECTION ( 'NONE',  ( 0.000000000000000000, 1.000000000000000000, 1.156482317317871478E-16 ) ) ;
#5901 = AXIS2_PLACEMENT_3D ( 'NONE', #4789, #4147, #7228 ) ;
#5902 = VERTEX_POINT ( 'NONE', #1854 ) ;
#5903 = DIRECTION ( 'NONE',  ( 1.000000000000000000, 0.000000000000000000, 0.000000000000000000 ) ) ;
#5904 = CARTESIAN_POINT ( 'NONE',  ( -26.99999999999998934, 1.959434878635763751E-16, -1.599999999999998979 ) ) ;
#5905 = EDGE_LOOP ( 'NONE', ( #5329, #5132, #4586, #86 ) ) ;
#5906 = PRESENTATION_LAYER_ASSIGNMENT (  '', '', ( #5579 ) ) ;
#5907 = CARTESIAN_POINT ( 'NONE',  ( -0.9046671180729963790, 5.711843387010016926, 13.57999999999999474 ) ) ;
#5908 = CARTESIAN_POINT ( 'NONE',  ( 2.496947748567516889, -4.900535883036019946, 3.639999999999999680 ) ) ;
#5909 = CARTESIAN_POINT ( 'NONE',  ( 5.432285873273257515, 0.8603895577212793411, 8.679999999999997939 ) ) ;
#5910 = EDGE_LOOP ( 'NONE', ( #6952, #8554, #2502, #2811 ) ) ;
#5911 = CARTESIAN_POINT ( 'NONE',  ( -0.6146835312500006365, -14.06466310670085562, -1.885416667349463227 ) ) ;
#5912 = ADVANCED_FACE ( 'NONE', ( #5814 ), #8170, .T. ) ;
#5913 = CIRCLE ( 'NONE', #8805, 3.000000000000000000 ) ;
#5914 = VECTOR ( 'NONE', #2883, 1000.000000000000000 ) ;
#5915 = ORIENTED_EDGE ( 'NONE', *, *, #541, .F. ) ;
#5916 = LINE ( 'NONE', #110, #8219 ) ;
#5917 = CARTESIAN_POINT ( 'NONE',  ( 1.300000000000000044, -0.7390083445627200209, 1.280000000000001137 ) ) ;
#5918 = ORIENTED_EDGE ( 'NONE', *, *, #5378, .T. ) ;
#5919 = CARTESIAN_POINT ( 'NONE',  ( 3.099999999999998757, 0.000000000000000000, 1.500000000000000222 ) ) ;
#5920 = CARTESIAN_POINT ( 'NONE',  ( -0.6146835312499998594, -11.93533689329915326, -1.677083334016129967 ) ) ;
#5921 = CARTESIAN_POINT ( 'NONE',  ( 3.244753828200538148, 3.119207202478391672, 7.403948283277976827 ) ) ;
#5922 = EDGE_LOOP ( 'NONE', ( #2253, #6221, #5380, #8110 ) ) ;
#5923 = VECTOR ( 'NONE', #6102, 1000.000000000000000 ) ;
#5924 = CARTESIAN_POINT ( 'NONE',  ( 0.000000000000000000, -13.00000000000000533, 0.000000000000000000 ) ) ;
#5925 = PRESENTATION_LAYER_ASSIGNMENT (  '', '', ( #8647 ) ) ;
#5926 = CARTESIAN_POINT ( 'NONE',  ( -0.9046671180729963790, 5.711843387010016926, 13.57999999999999474 ) ) ;
#5927 = VECTOR ( 'NONE', #6273, 1000.000000000000000 ) ;
#5928 = CARTESIAN_POINT ( 'NONE',  ( 0.000000000000000000, -7.750000000000000000, -12.00000000000000000 ) ) ;
#5929 = CARTESIAN_POINT ( 'NONE',  ( -0.9046671180729962680, 5.711843387010016926, 7.979999999999999538 ) ) ;
#5930 = AXIS2_PLACEMENT_3D ( 'NONE', #9266, #1307, #3642 ) ;
#5931 = DIRECTION ( 'NONE',  ( 0.000000000000000000, -0.4999999999999991118, 0.8660254037844391517 ) ) ;
#5932 = CARTESIAN_POINT ( 'NONE',  ( 10.00000000000000000, 1.459547570502460978, -6.894905428400257996 ) ) ;
#5933 = AXIS2_PLACEMENT_3D ( 'NONE', #9949, #9041, #9742 ) ;
#5934 = CARTESIAN_POINT ( 'NONE',  ( 0.1499999999999973577, 3.367778697655221012E-16, -2.750000000000000000 ) ) ;
#5935 = CARTESIAN_POINT ( 'NONE',  ( -0.6162731882459178134, -4.458484982038665834, 13.31605171672202204 ) ) ;
#5936 = CARTESIAN_POINT ( 'NONE',  ( 1.229367062500000163, -13.00000000000000533, -1.218750000682796486 ) ) ;
#5937 = CARTESIAN_POINT ( 'NONE',  ( 4.023224611898322145, -4.155232146225737111, 2.503948283277976472 ) ) ;
#5938 = CARTESIAN_POINT ( 'NONE',  ( 1.229367062500000163, -13.70977540446723886, -1.260416667349463449 ) ) ;
#5939 = ORIENTED_EDGE ( 'NONE', *, *, #6284, .T. ) ;
#5940 = CARTESIAN_POINT ( 'NONE',  ( -3.826313983664925811, -3.951860609387098489, 2.396051716722022551 ) ) ;
#5941 = DIRECTION ( 'NONE',  ( 0.000000000000000000, 0.000000000000000000, -1.000000000000000000 ) ) ;
#5942 = CARTESIAN_POINT ( 'NONE',  ( 10.00000000000000000, 0.000000000000000000, 0.000000000000000000 ) ) ;
#5943 = ORIENTED_EDGE ( 'NONE', *, *, #9694, .F. ) ;
#5944 = EDGE_CURVE ( 'NONE', #9543, #5109, #4127, .T. ) ;
#5945 = CARTESIAN_POINT ( 'NONE',  ( -0.7039550926810301812, -4.444597532678121965, 6.719999999999999751 ) ) ;
#5946 = CARTESIAN_POINT ( 'NONE',  ( -4.673326407553653361, 0.7401821875142517992, 4.620000000000000107 ) ) ;
#5947 = CARTESIAN_POINT ( 'NONE',  ( -1.229367062500000163, -12.29022459553277002, -2.135416667349463449 ) ) ;
#5948 = ORIENTED_EDGE ( 'NONE', *, *, #8031, .T. ) ;
#5949 = DIRECTION ( 'NONE',  ( -1.000000000000000000, 0.000000000000000000, 6.123233995736766036E-17 ) ) ;
#5950 = ORIENTED_EDGE ( 'NONE', *, *, #1512, .T. ) ;
#5951 = DIRECTION ( 'NONE',  ( 0.000000000000000000, 0.000000000000000000, 1.000000000000000000 ) ) ;
#5952 = CARTESIAN_POINT ( 'NONE',  ( 5.999999999999999112, -27.00000000000000711, -14.00000000000000178 ) ) ;
#5953 = ORIENTED_EDGE ( 'NONE', *, *, #9762, .F. ) ;
#5954 = EDGE_CURVE ( 'NONE', #9536, #10476, #5916, .T. ) ;
#5955 = CARTESIAN_POINT ( 'NONE',  ( -4.900535883036028828, 2.496947748567499126, 10.35999999999999943 ) ) ;
#5956 = EDGE_CURVE ( 'NONE', #3378, #4582, #1908, .T. ) ;
#5957 = CARTESIAN_POINT ( 'NONE',  ( 0.9046671180729951578, -5.711843387010016926, 3.779999999999998472 ) ) ;
#5958 = CARTESIAN_POINT ( 'NONE',  ( -4.089228379062038066, 4.089228379062021190, 7.699999999999998401 ) ) ;
#5959 = ORIENTED_EDGE ( 'NONE', *, *, #7937, .T. ) ;
#5960 = CARTESIAN_POINT ( 'NONE',  ( 0.6146835312499993043, -14.06466310670085562, -0.8020833340161299674 ) ) ;
#5961 = VECTOR ( 'NONE', #1607, 1000.000000000000000 ) ;
#5962 =( NAMED_UNIT ( * ) PLANE_ANGLE_UNIT ( ) SI_UNIT ( $, .RADIAN. ) );
#5963 = ORIENTED_EDGE ( 'NONE', *, *, #9940, .T. ) ;
#5964 = CARTESIAN_POINT ( 'NONE',  ( 9.869213319667256457, 3.750000000000000000, 0.000000000000000000 ) ) ;
#5965 = LINE ( 'NONE', #3443, #4390 ) ;
#5966 = ORIENTED_EDGE ( 'NONE', *, *, #2682, .F. ) ;
#5967 = ADVANCED_FACE ( 'NONE', ( #6563 ), #5129, .T. ) ;
#5968 = LINE ( 'NONE', #1962, #10160 ) ;
#5969 = CARTESIAN_POINT ( 'NONE',  ( 8.000000000000001776, -7.009698679648292519, 0.7308381473896652381 ) ) ;
#5970 = VECTOR ( 'NONE', #8286, 1000.000000000000114 ) ;
#5971 = CARTESIAN_POINT ( 'NONE',  ( -0.6146835312499998594, -11.93533689329915326, -0.1770833340161300506 ) ) ;
#5972 = CARTESIAN_POINT ( 'NONE',  ( 4.658724279160018966, -0.8323763977770426425, 10.62394828327797569 ) ) ;
#5973 = EDGE_LOOP ( 'NONE', ( #5440, #4967, #515, #4437 ) ) ;
#5974 = CYLINDRICAL_SURFACE ( 'NONE', #4406, 3.000000000000000000 ) ;
#5975 = DIRECTION ( 'NONE',  ( -1.000000000000000000, -2.312964634635742957E-16, 0.000000000000000000 ) ) ;
#5976 = CARTESIAN_POINT ( 'NONE',  ( -15.00000000000000000, 19.99999999999999645, 9.000000000000000000 ) ) ;
#5977 = VECTOR ( 'NONE', #10041, 1000.000000000000000 ) ;
#5978 = CARTESIAN_POINT ( 'NONE',  ( 0.8603895577212593571, 5.432285873273261068, 8.119999999999999218 ) ) ;
#5979 = DIRECTION ( 'NONE',  ( -1.000000000000000000, 0.000000000000000000, -0.000000000000000000 ) ) ;
#5980 = DIRECTION ( 'NONE',  ( 0.000000000000000000, 0.000000000000000000, -1.000000000000000000 ) ) ;
#5981 = CARTESIAN_POINT ( 'NONE',  ( -1.500000000000000222, -13.00000000000000533, -0.7500000000000002220 ) ) ;
#5982 = CARTESIAN_POINT ( 'NONE',  ( -4.430710083317573655, -0.7916369971161599794, 13.87605171672202253 ) ) ;
#5983 = CARTESIAN_POINT ( 'NONE',  ( 1.229367062500000385, -12.29022459553277002, -2.677083334016129967 ) ) ;
#5984 = AXIS2_PLACEMENT_3D ( 'NONE', #1018, #4296, #285 ) ;
#5985 = CARTESIAN_POINT ( 'NONE',  ( -0.6479879772514802738, 4.687928535947285091, 12.58394828327797477 ) ) ;
#5986 = CARTESIAN_POINT ( 'NONE',  ( -0.6146835312500006365, -14.06466310670085562, 0.1145833326505365929 ) ) ;
#5987 = CIRCLE ( 'NONE', #10085, 2.399999999999999911 ) ;
#5988 = APPLICATION_CONTEXT ( 'automotive_design' ) ;
#5989 = EDGE_LOOP ( 'NONE', ( #2691, #304, #5571, #2054 ) ) ;
#5990 = CARTESIAN_POINT ( 'NONE',  ( -4.155232146225753098, 4.023224611898306158, 8.696051716722022817 ) ) ;
#5991 = DIRECTION ( 'NONE',  ( 0.000000000000000000, 0.000000000000000000, -1.000000000000000000 ) ) ;
#5992 = CARTESIAN_POINT ( 'NONE',  ( 0.000000000000000000, 0.000000000000000000, 2.600000000000000089 ) ) ;
#5993 = EDGE_LOOP ( 'NONE', ( #8998, #4389, #4737, #5085 ) ) ;
#5994 = VECTOR ( 'NONE', #4216, 1000.000000000000000 ) ;
#5995 = CARTESIAN_POINT ( 'NONE',  ( 3.345732310141667387, -3.345732310141654064, 9.099999999999996092 ) ) ;
#5996 = EDGE_CURVE ( 'NONE', #8355, #6611, #5813, .T. ) ;
#5997 = FILL_AREA_STYLE_COLOUR ( '', #8308 ) ;
#5998 = CARTESIAN_POINT ( 'NONE',  ( 3.181980515339458471, 3.181980515339470461, 2.799999999999999378 ) ) ;
#5999 = CARTESIAN_POINT ( 'NONE',  ( 1.229367062500000385, -12.29022459553277002, -0.8020833340161301894 ) ) ;
#6000 = ORIENTED_EDGE ( 'NONE', *, *, #7626, .F. ) ;
#6001 = CARTESIAN_POINT ( 'NONE',  ( -1.836970198721029688E-16, 0.000000000000000000, -33.00000000000000711 ) ) ;
#6002 = VECTOR ( 'NONE', #8819, 1000.000000000000000 ) ;
#6003 = EDGE_CURVE ( 'NONE', #3335, #4690, #5233, .T. ) ;
#6004 = VERTEX_POINT ( 'NONE', #368 ) ;
#6005 = CARTESIAN_POINT ( 'NONE',  ( 1.500000000000000222, -13.00000000000000533, -0.5000000000000000000 ) ) ;
#6006 = VECTOR ( 'NONE', #8185, 1000.000000000000000 ) ;
#6007 = CARTESIAN_POINT ( 'NONE',  ( 0.1499999999999973577, 3.184081677783118191E-16, -2.600000000000000089 ) ) ;
#6008 = ORIENTED_EDGE ( 'NONE', *, *, #5254, .T. ) ;
#6009 = CARTESIAN_POINT ( 'NONE',  ( -2.625446233515515981, -5.152728359536500768, 9.659999999999994813 ) ) ;
#6010 = CARTESIAN_POINT ( 'NONE',  ( -5.711843387010018702, 0.9046671180729746187, 10.21999999999999709 ) ) ;
#6011 = CARTESIAN_POINT ( 'NONE',  ( -0.8603895577212598011, -5.432285873273260179, 12.31999999999999851 ) ) ;
#6012 = VERTEX_POINT ( 'NONE', #6820 ) ;
#6013 = AXIS2_PLACEMENT_3D ( 'NONE', #2022, #6032, #5400 ) ;
#6014 = DIRECTION ( 'NONE',  ( 0.000000000000000000, 0.000000000000000000, -1.000000000000000000 ) ) ;
#6015 = AXIS2_PLACEMENT_3D ( 'NONE', #3288, #2449, #2603 ) ;
#6016 = EDGE_CURVE ( 'NONE', #3392, #2266, #3646, .T. ) ;
#6017 = EDGE_CURVE ( 'NONE', #9702, #10315, #3694, .T. ) ;
#6018 = EDGE_LOOP ( 'NONE', ( #3990, #6126, #7484, #8436 ) ) ;
#6019 = PLANE ( 'NONE',  #9411 ) ;
#6020 = DIRECTION ( 'NONE',  ( 0.000000000000000000, -1.000000000000000000, -0.000000000000000000 ) ) ;
#6021 = VERTEX_POINT ( 'NONE', #8479 ) ;
#6022 = DIRECTION ( 'NONE',  ( 0.000000000000000000, 0.000000000000000000, 1.000000000000000000 ) ) ;
#6023 = CARTESIAN_POINT ( 'NONE',  ( 15.00000000000000000, 19.99999999999999645, -9.000000000000000000 ) ) ;
#6024 = DIRECTION ( 'NONE',  ( 1.000000000000000000, 0.000000000000000000, -0.000000000000000000 ) ) ;
#6025 = CARTESIAN_POINT ( 'NONE',  ( 0.8124729078102063129, -5.726445515403652209, -0.01605171672202330979 ) ) ;
#6026 = VERTEX_POINT ( 'NONE', #315 ) ;
#6027 = CARTESIAN_POINT ( 'NONE',  ( -2.000000000000000000, 0.000000000000000000, 0.000000000000000000 ) ) ;
#6028 = DIRECTION ( 'NONE',  ( -1.000000000000000000, 0.000000000000000000, 0.000000000000000000 ) ) ;
#6029 = EDGE_CURVE ( 'NONE', #4105, #6004, #1617, .T. ) ;
#6030 = CARTESIAN_POINT ( 'NONE',  ( -29.99999999999998934, -13.00000000000000533, 0.000000000000000000 ) ) ;
#6031 = CARTESIAN_POINT ( 'NONE',  ( -0.7499999999999997780, -11.70096189432334555, -2.833333333333333481 ) ) ;
#6032 = DIRECTION ( 'NONE',  ( 0.000000000000000000, 0.000000000000000000, 1.000000000000000000 ) ) ;
#6033 = CARTESIAN_POINT ( 'NONE',  ( 8.000000000000001776, 3.771202944355774189, -4.982773259188334691 ) ) ;
#6034 = CARTESIAN_POINT ( 'NONE',  ( -2.399999999999999911, 0.000000000000000000, 6.999999999999999112 ) ) ;
#6035 = CARTESIAN_POINT ( 'NONE',  ( 0.8323763977770604061, -4.658724279160015413, 13.17605171672201969 ) ) ;
#6036 = CARTESIAN_POINT ( 'NONE',  ( 8.692241771943169307E-17, -11.58044919106553294, -1.093750000682796486 ) ) ;
#6037 = CARTESIAN_POINT ( 'NONE',  ( -2.708615832122950096, -5.110351332421780413, 3.063948283277976081 ) ) ;
#6038 = EDGE_CURVE ( 'NONE', #4888, #1744, #1364, .T. ) ;
#6039 = CARTESIAN_POINT ( 'NONE',  ( -1.229367062500000163, -13.70977540446723708, -0.4270833340161298564 ) ) ;
#6040 = ORIENTED_EDGE ( 'NONE', *, *, #3124, .T. ) ;
#6041 = CARTESIAN_POINT ( 'NONE',  ( 0.000000000000000000, 26.99999999999999289, 0.000000000000000000 ) ) ;
#6042 = FACE_OUTER_BOUND ( 'NONE', #5989, .T. ) ;
#6043 = DIRECTION ( 'NONE',  ( -1.156482317317871478E-16, 1.000000000000000000, 0.000000000000000000 ) ) ;
#6044 = LINE ( 'NONE', #8407, #3062 ) ;
#6045 = ORIENTED_EDGE ( 'NONE', *, *, #3498, .F. ) ;
#6046 = CARTESIAN_POINT ( 'NONE',  ( 0.7401821875142697849, -4.673326407553650697, 6.579999999999999183 ) ) ;
#6047 = DIRECTION ( 'NONE',  ( -1.000000000000000000, -0.000000000000000000, 0.000000000000000000 ) ) ;
#6048 = CARTESIAN_POINT ( 'NONE',  ( 4.444597532678119300, 0.7039550926810472786, 5.879999999999999893 ) ) ;
#6049 = CARTESIAN_POINT ( 'NONE',  ( 1.229367062500000163, -13.00000000000000533, -1.343750000682796486 ) ) ;
#6050 = VERTEX_POINT ( 'NONE', #8429 ) ;
#6051 = FILL_AREA_STYLE_COLOUR ( '', #7540 ) ;
#6052 = ORIENTED_EDGE ( 'NONE', *, *, #2934, .F. ) ;
#6053 = EDGE_CURVE ( 'NONE', #118, #3161, #1782, .T. ) ;
#6054 = DIRECTION ( 'NONE',  ( 1.000000000000000000, 0.000000000000000000, 0.000000000000000000 ) ) ;
#6055 = CARTESIAN_POINT ( 'NONE',  ( 1.999999999999975797, 15.00000000000000355, 6.000000000000010658 ) ) ;
#6056 = LINE ( 'NONE', #8468, #10003 ) ;
#6057 = ORIENTED_EDGE ( 'NONE', *, *, #4526, .F. ) ;
#6058 = CARTESIAN_POINT ( 'NONE',  ( 3.889087296526005488, 3.889087296526018811, 13.99999999999999822 ) ) ;
#6059 = VECTOR ( 'NONE', #2450, 1000.000000000000000 ) ;
#6060 = CARTESIAN_POINT ( 'NONE',  ( -5.432285873273256627, -0.8603895577212797852, 12.87999999999999901 ) ) ;
#6061 = CARTESIAN_POINT ( 'NONE',  ( -5.152728359536494551, -2.625446233515535077, 9.939999999999994174 ) ) ;
#6062 = EDGE_LOOP ( 'NONE', ( #1207, #4374 ) ) ;
#6063 = CARTESIAN_POINT ( 'NONE',  ( -2.000000000000000000, 5.904264776415100613, 2.046865518294722630 ) ) ;
#6064 = ADVANCED_FACE ( 'NONE', ( #6181 ), #6019, .T. ) ;
#6065 = UNCERTAINTY_MEASURE_WITH_UNIT (LENGTH_MEASURE( 1.000000000000000082E-05 ), #2782, 'distance_accuracy_value', 'NONE');
#6066 =( REPRESENTATION_RELATIONSHIP ('NONE','NONE', #5100, #9430 ) REPRESENTATION_RELATIONSHIP_WITH_TRANSFORMATION ( #6522 )SHAPE_REPRESENTATION_RELATIONSHIP( ) );
#6067 = SURFACE_STYLE_USAGE ( .BOTH. , #2907 ) ;
#6068 = VECTOR ( 'NONE', #1887, 1000.000000000000000 ) ;
#6069 = ORIENTED_EDGE ( 'NONE', *, *, #457, .F. ) ;
#6070 = CARTESIAN_POINT ( 'NONE',  ( 11.00000000000000355, 0.000000000000000000, 0.000000000000000000 ) ) ;
#6071 = CIRCLE ( 'NONE', #8459, 3.000000000000000000 ) ;
#6072 = DIRECTION ( 'NONE',  ( 0.000000000000000000, 0.000000000000000000, 1.000000000000000000 ) ) ;
#6073 = ORIENTED_EDGE ( 'NONE', *, *, #5117, .T. ) ;
#6074 = CARTESIAN_POINT ( 'NONE',  ( 8.000000000000001776, -1.471047635026825784, -6.892461014225975013 ) ) ;
#6075 = CIRCLE ( 'NONE', #672, 3.000000000000000000 ) ;
#6076 = DIRECTION ( 'NONE',  ( 0.3420201433256627732, -0.9396926207859105373, 0.000000000000000000 ) ) ;
#6077 = DIRECTION ( 'NONE',  ( 0.000000000000000000, 0.000000000000000000, -1.000000000000000000 ) ) ;
#6078 = CARTESIAN_POINT ( 'NONE',  ( 4.458484982038663169, 0.6162731882459350219, 10.48394828327797512 ) ) ;
#6079 = ORIENTED_EDGE ( 'NONE', *, *, #671, .T. ) ;
#6080 = VECTOR ( 'NONE', #9973, 1000.000000000000000 ) ;
#6081 = DIRECTION ( 'NONE',  ( -0.000000000000000000, -0.000000000000000000, 1.000000000000000000 ) ) ;
#6082 = EDGE_CURVE ( 'NONE', #1984, #980, #9436, .T. ) ;
#6083 = VECTOR ( 'NONE', #551, 1000.000000000000000 ) ;
#6084 = CARTESIAN_POINT ( 'NONE',  ( -5.432285873273256627, -0.8603895577212797852, 12.87999999999999901 ) ) ;
#6085 = DIRECTION ( 'NONE',  ( 0.000000000000000000, 0.000000000000000000, 1.000000000000000000 ) ) ;
#6086 = CARTESIAN_POINT ( 'NONE',  ( 1.530808498934188612E-16, -19.00000000000000711, 1.249999999999997558 ) ) ;
#6087 = VECTOR ( 'NONE', #10064, 1000.000000000000000 ) ;
#6088 = DIRECTION ( 'NONE',  ( -1.000000000000000000, -0.000000000000000000, -0.000000000000000000 ) ) ;
#6089 = VECTOR ( 'NONE', #7043, 1000.000000000000000 ) ;
#6090 = VECTOR ( 'NONE', #1373, 1000.000000000000000 ) ;
#6091 = DIRECTION ( 'NONE',  ( -1.000000000000000000, -0.000000000000000000, 0.000000000000000000 ) ) ;
#6092 = CARTESIAN_POINT ( 'NONE',  ( -4.049832306626335310, 1.963858260114700327, 14.15605171672202012 ) ) ;
#6093 = EDGE_CURVE ( 'NONE', #525, #7355, #5000, .T. ) ;
#6094 = EDGE_CURVE ( 'NONE', #8717, #9974, #1154, .T. ) ;
#6095 = CARTESIAN_POINT ( 'NONE',  ( 1.229367062500000163, -13.00000000000000533, -0.7187500006827964860 ) ) ;
#6096 = AXIS2_PLACEMENT_3D ( 'NONE', #3286, #6511, #8171 ) ;
#6097 = AXIS2_PLACEMENT_3D ( 'NONE', #7447, #3469, #6694 ) ;
#6098 = CARTESIAN_POINT ( 'NONE',  ( 5.446173322633801384, 0.7727076532861675284, 2.083948283277976543 ) ) ;
#6099 = CARTESIAN_POINT ( 'NONE',  ( -0.6146835312500006365, -14.06466310670085562, -0.8854166673494632267 ) ) ;
#6101 = VERTEX_POINT ( 'NONE', #5964 ) ;
#6100 = AXIS2_PLACEMENT_3D ( 'NONE', #2263, #2317, #669 ) ;
#6102 = DIRECTION ( 'NONE',  ( 5.204170427930421283E-15, 6.018531076210112041E-31, 1.000000000000000000 ) ) ;
#6103 = AXIS2_PLACEMENT_3D ( 'NONE', #9140, #1082, #4108 ) ;
#6104 = LINE ( 'NONE', #9407, #2222 ) ;
#6105 = CARTESIAN_POINT ( 'NONE',  ( 0.000000000000000000, -27.00000000000000711, -1.249999999999988898 ) ) ;
#6106 = FACE_OUTER_BOUND ( 'NONE', #607, .T. ) ;
#6107 = ORIENTED_EDGE ( 'NONE', *, *, #5143, .F. ) ;
#6108 = EDGE_CURVE ( 'NONE', #10253, #8513, #4150, .T. ) ;
#6109 = CARTESIAN_POINT ( 'NONE',  ( 0.7039550926810297371, 4.444597532678122853, 13.71999999999999886 ) ) ;
#6110 = CARTESIAN_POINT ( 'NONE',  ( -4.687928535947287756, 0.6479879772514611780, 14.01605171672202310 ) ) ;
#6111 = CARTESIAN_POINT ( 'NONE',  ( -1.500000000000000222, -13.00000000000000533, -2.750000000000000000 ) ) ;
#6112 = ORIENTED_EDGE ( 'NONE', *, *, #7138, .F. ) ;
#6113 = VERTEX_POINT ( 'NONE', #1959 ) ;
#6114 = CARTESIAN_POINT ( 'NONE',  ( 17.00000000000000000, 19.99999999999999645, 6.000000000000000000 ) ) ;
#6115 = LINE ( 'NONE', #218, #25 ) ;
#6116 = CARTESIAN_POINT ( 'NONE',  ( -2.000000000000000000, -5.979767908488829775, -1.814490771706245065 ) ) ;
#6117 = ORIENTED_EDGE ( 'NONE', *, *, #4455, .T. ) ;
#6118 = CARTESIAN_POINT ( 'NONE',  ( -5.418398423912711870, -0.9480714621563917088, 5.476051716722023066 ) ) ;
#6119 = CARTESIAN_POINT ( 'NONE',  ( 4.089228379062037178, -4.089228379062022967, 11.90000000000000036 ) ) ;
#6120 = CARTESIAN_POINT ( 'NONE',  ( 5.019816903233806471, -10.00000000000000000, 0.000000000000000000 ) ) ;
#6121 = ORIENTED_EDGE ( 'NONE', *, *, #5820, .F. ) ;
#6122 = CARTESIAN_POINT ( 'NONE',  ( 10.00000000000000000, -5.522688772756355391, -6.461416928141300531 ) ) ;
#6123 = PRODUCT_DEFINITION ( 'UNKNOWN', '', #3808, #2415 ) ;
#6124 = ORIENTED_EDGE ( 'NONE', *, *, #5311, .T. ) ;
#6125 =( LENGTH_UNIT ( ) NAMED_UNIT ( * ) SI_UNIT ( .MILLI., .METRE. ) );
#6126 = ORIENTED_EDGE ( 'NONE', *, *, #5895, .T. ) ;
#6127 = CARTESIAN_POINT ( 'NONE',  ( 0.000000000000000000, 0.000000000000000000, 9.000000000000000000 ) ) ;
#6128 = LINE ( 'NONE', #3798, #9143 ) ;
#6129 = ORIENTED_EDGE ( 'NONE', *, *, #6252, .T. ) ;
#6130 = CARTESIAN_POINT ( 'NONE',  ( 1.300000000000000044, 1.478016689125442484, -1.626303258728256651E-15 ) ) ;
#6131 = DIRECTION ( 'NONE',  ( 0.3420201433256627732, 0.9396926207859105373, 0.000000000000000000 ) ) ;
#6132 = CARTESIAN_POINT ( 'NONE',  ( -4.258245684917310925, -2.064922774268914019, 8.943948283277975975 ) ) ;
#6133 = ORIENTED_EDGE ( 'NONE', *, *, #7193, .F. ) ;
#6134 = DIRECTION ( 'NONE',  ( 1.000000000000000000, 0.000000000000000000, 0.000000000000000000 ) ) ;
#6135 = APPLICATION_CONTEXT ( 'automotive_design' ) ;
#6136 = AXIS2_PLACEMENT_3D ( 'NONE', #9332, #627, #474 ) ;
#6137 = CARTESIAN_POINT ( 'NONE',  ( 1.500000000000000222, -13.00000000000000533, -0.5625000013655934161 ) ) ;
#6138 = LINE ( 'NONE', #8491, #4973 ) ;
#6139 = CYLINDRICAL_SURFACE ( 'NONE', #428, 1.500000000000000222 ) ;
#6140 = EDGE_CURVE ( 'NONE', #8424, #9096, #2850, .T. ) ;
#6141 = DIRECTION ( 'NONE',  ( -1.000000000000000000, -0.000000000000000000, -0.000000000000000000 ) ) ;
#6142 = VECTOR ( 'NONE', #184, 1000.000000000000000 ) ;
#6143 = LINE ( 'NONE', #2128, #7209 ) ;
#6144 = DIRECTION ( 'NONE',  ( 0.000000000000000000, 0.000000000000000000, 1.000000000000000000 ) ) ;
#6145 = LINE ( 'NONE', #8546, #5386 ) ;
#6146 = CARTESIAN_POINT ( 'NONE',  ( 4.673326407553653361, -0.7401821875142523544, 0.4199999999999999845 ) ) ;
#6147 = CARTESIAN_POINT ( 'NONE',  ( 0.6146835312500001924, -11.93533689329915326, -2.260416667349463449 ) ) ;
#6148 = CARTESIAN_POINT ( 'NONE',  ( 5.446173322633801384, 0.7727076532861675284, -0.7160517167220232793 ) ) ;
#6149 = CARTESIAN_POINT ( 'NONE',  ( -1.229367062500000163, -13.00000000000000533, -1.968750000682796708 ) ) ;
#6150 = ORIENTED_EDGE ( 'NONE', *, *, #8229, .F. ) ;
#6151 = ADVANCED_FACE ( 'NONE', ( #2802 ), #5160, .T. ) ;
#6152 = CARTESIAN_POINT ( 'NONE',  ( 2.697157280332745266, 3.750000000000000000, -12.00000000000000000 ) ) ;
#6153 = EDGE_CURVE ( 'NONE', #8450, #6050, #8530, .T. ) ;
#6154 =( BOUNDED_CURVE ( )  B_SPLINE_CURVE ( 2, ( #3176, #5164, #6648, #3370, #4166, #938, #987 ),
 .UNSPECIFIED., .F., .T. ) 
 B_SPLINE_CURVE_WITH_KNOTS ( ( 3, 2, 2, 3 ),
 ( 0.4166666666666666297, 0.4444444444444443643, 0.4722222222222222099, 0.5000000000000000000 ),
 .UNSPECIFIED. ) 
 CURVE ( )  GEOMETRIC_REPRESENTATION_ITEM ( )  RATIONAL_B_SPLINE_CURVE ( ( 1.000000000000000222, 0.8660254037844384856, 1.000000000000000000, 0.8660254037844387076, 1.000000000000000000, 0.8660254037844387076, 1.000000000000000000 ) ) 
 REPRESENTATION_ITEM ( '' )  );
#6155 = LINE ( 'NONE', #1446, #7976 ) ;
#6156 = LINE ( 'NONE', #3723, #10192 ) ;
#6157 = CARTESIAN_POINT ( 'NONE',  ( 1.868979409283444415, -10.02539999999999942, -12.00000000000000000 ) ) ;
#6158 = ORIENTED_EDGE ( 'NONE', *, *, #5420, .F. ) ;
#6159 = CARTESIAN_POINT ( 'NONE',  ( 0.000000000000000000, 18.99999999999999289, 0.000000000000000000 ) ) ;
#6160 = CARTESIAN_POINT ( 'NONE',  ( -13.00000000000000000, 19.99999999999999645, -9.000000000000000000 ) ) ;
#6161 = CARTESIAN_POINT ( 'NONE',  ( 4.009529358847659708, -2.042957248827953709, 0.5599999999999999423 ) ) ;
#6162 = CARTESIAN_POINT ( 'NONE',  ( -1.229367062500000385, -13.70977540446723886, -0.5520833340161299674 ) ) ;
#6163 = MECHANICAL_DESIGN_GEOMETRIC_PRESENTATION_REPRESENTATION (  '', ( #259 ), #4138 ) ;
#6164 = VERTEX_POINT ( 'NONE', #7734 ) ;
#6165 = ADVANCED_FACE ( 'NONE', ( #6921, #6977, #2909 ), #2113, .T. ) ;
#6166 = VERTEX_POINT ( 'NONE', #8581 ) ;
#6167 = CARTESIAN_POINT ( 'NONE',  ( 2.500000000000000000, 3.061616997868383141E-16, 3.000000000000000000 ) ) ;
#6168 = VECTOR ( 'NONE', #7627, 1000.000000000000000 ) ;
#6169 = CARTESIAN_POINT ( 'NONE',  ( 25.00000000000000000, -4.000000000000000000, 0.000000000000000000 ) ) ;
#6170 = ORIENTED_EDGE ( 'NONE', *, *, #6969, .T. ) ;
#6171 = CARTESIAN_POINT ( 'NONE',  ( 0.7727076532861471003, 5.446173322633805824, 9.116051716722020970 ) ) ;
#6172 =( GEOMETRIC_REPRESENTATION_CONTEXT ( 3 ) GLOBAL_UNCERTAINTY_ASSIGNED_CONTEXT ( ( #4003 ) ) GLOBAL_UNIT_ASSIGNED_CONTEXT ( ( #5649, #3165, #4063 ) ) REPRESENTATION_CONTEXT ( 'NONE', 'WORKASPACE' ) );
#6173 = FILL_AREA_STYLE ('',( #4530 ) ) ;
#6174 = ORIENTED_EDGE ( 'NONE', *, *, #9678, .F. ) ;
#6175 = PLANE ( 'NONE',  #1888 ) ;
#6176 = AXIS2_PLACEMENT_3D ( 'NONE', #6127, #4536, #5338 ) ;
#6177 = ORIENTED_EDGE ( 'NONE', *, *, #7866, .F. ) ;
#6178 = EDGE_CURVE ( 'NONE', #4919, #8624, #2798, .T. ) ;
#6179 = AXIS2_PLACEMENT_3D ( 'NONE', #6899, #9297, #5363 ) ;
#6180 = ORIENTED_EDGE ( 'NONE', *, *, #2488, .F. ) ;
#6181 = FACE_OUTER_BOUND ( 'NONE', #8853, .T. ) ;
#6182 = CARTESIAN_POINT ( 'NONE',  ( 22.43558391966725907, 3.750000000000000000, -12.00000000000000000 ) ) ;
#6183 = EDGE_LOOP ( 'NONE', ( #4909, #8985 ) ) ;
#6184 = CARTESIAN_POINT ( 'NONE',  ( 19.29399126966725575, 3.750000000000000000, 0.000000000000000000 ) ) ;
#6185 = AXIS2_PLACEMENT_3D ( 'NONE', #7584, #2712, #5931 ) ;
#6186 = CARTESIAN_POINT ( 'NONE',  ( 10.00000000000000000, -6.700937042937042065, 0.8165525598867396928 ) ) ;
#6187 = CARTESIAN_POINT ( 'NONE',  ( -5.697241258616385196, 0.9968613283357647958, 6.423948283277978177 ) ) ;
#6188 = ORIENTED_EDGE ( 'NONE', *, *, #4277, .T. ) ;
#6189 = AXIS2_PLACEMENT_3D ( 'NONE', #4400, #7586, #3609 ) ;
#6190 = DIRECTION ( 'NONE',  ( -1.000000000000000000, -0.000000000000000000, -0.000000000000000000 ) ) ;
#6191 = CARTESIAN_POINT ( 'NONE',  ( -1.500000000000000222, -13.00000000000000533, -3.000000000000000000 ) ) ;
#6192 = CARTESIAN_POINT ( 'NONE',  ( 1.300000000000000044, -0.7390083445627200209, 1.280000000000001137 ) ) ;
#6193 = CARTESIAN_POINT ( 'NONE',  ( 30.00000000000001066, 35.00000000000001421, -9.000000000000000000 ) ) ;
#6194 = DIRECTION ( 'NONE',  ( 1.000000000000000000, 0.000000000000000000, 0.000000000000000000 ) ) ;
#6195 = DIRECTION ( 'NONE',  ( -0.9396926207859105373, 0.3420201433256627732, 0.000000000000000000 ) ) ;
#6196 = EDGE_CURVE ( 'NONE', #4172, #8945, #7834, .T. ) ;
#6197 = CARTESIAN_POINT ( 'NONE',  ( -1.500000000000003775, -13.86602540378444104, -1.208333333333333703 ) ) ;
#6198 = CARTESIAN_POINT ( 'NONE',  ( 30.00000000000001066, -34.99999999999999289, -9.000000000000000000 ) ) ;
#6199 = CARTESIAN_POINT ( 'NONE',  ( 4.444597532678119300, 0.7039550926810472786, 3.079999999999999627 ) ) ;
#6200 = CARTESIAN_POINT ( 'NONE',  ( 1.229367062500000163, -13.00000000000000533, -2.843750000682796486 ) ) ;
#6201 = ADVANCED_FACE ( 'NONE', ( #10282 ), #10394, .F. ) ;
#6202 = CARTESIAN_POINT ( 'NONE',  ( -4.023224611898323033, 4.155232146225737111, 9.503948283277974696 ) ) ;
#6203 = CARTESIAN_POINT ( 'NONE',  ( 11.29375735928344504, 6.025400000000000311, -12.00000000000000000 ) ) ;
#6204 = ORIENTED_EDGE ( 'NONE', *, *, #6377, .F. ) ;
#6205 = CARTESIAN_POINT ( 'NONE',  ( 1.500000000000000222, -13.00000000000000533, -2.062500001365593416 ) ) ;
#6206 = DIRECTION ( 'NONE',  ( -0.000000000000000000, 1.000000000000000000, -0.000000000000000000 ) ) ;
#6207 = DIRECTION ( 'NONE',  ( 1.000000000000000000, 0.000000000000000000, -0.000000000000000000 ) ) ;
#6208 = CARTESIAN_POINT ( 'NONE',  ( -2.000000000000000000, -3.573533178329545645, -5.126388750707257635 ) ) ;
#6209 = VERTEX_POINT ( 'NONE', #5602 ) ;
#6210 = CARTESIAN_POINT ( 'NONE',  ( -2.000000000000000000, 0.000000000000000000, 0.000000000000000000 ) ) ;
#6211 = CARTESIAN_POINT ( 'NONE',  ( -4.673326407553653361, 0.7401821875142517992, 10.21999999999999709 ) ) ;
#6212 = EDGE_CURVE ( 'NONE', #144, #9930, #8894, .T. ) ;
#6213 = CARTESIAN_POINT ( 'NONE',  ( 8.692241771943169307E-17, -11.58044919106553294, -1.718750000682796708 ) ) ;
#6214 = VERTEX_POINT ( 'NONE', #7939 ) ;
#6215 = ORIENTED_EDGE ( 'NONE', *, *, #7254, .F. ) ;
#6216 = CARTESIAN_POINT ( 'NONE',  ( 4.404961046766194599, 6.000000000000000000, -12.00000000000000000 ) ) ;
#6217 = CARTESIAN_POINT ( 'NONE',  ( 1.060575238724907038E-16, -11.26794919243112680, -2.437500001365593860 ) ) ;
#6218 = VERTEX_POINT ( 'NONE', #5492 ) ;
#6219 = CARTESIAN_POINT ( 'NONE',  ( 2.542276634908080535, 5.195105386651229118, 6.456051716722022604 ) ) ;
#6220 = CARTESIAN_POINT ( 'NONE',  ( 10.00000000000000000, -7.063614741696270016, 8.843061888689529582 ) ) ;
#6221 = ORIENTED_EDGE ( 'NONE', *, *, #5886, .F. ) ;
#6222 = EDGE_CURVE ( 'NONE', #1785, #6919, #1586, .T. ) ;
#6223 = EDGE_CURVE ( 'NONE', #3693, #2633, #2432, .T. ) ;
#6224 = CARTESIAN_POINT ( 'NONE',  ( 0.000000000000000000, 0.000000000000000000, 0.000000000000000000 ) ) ;
#6225 = VERTEX_POINT ( 'NONE', #6285 ) ;
#6226 = VERTEX_POINT ( 'NONE', #2374 ) ;
#6227 = CARTESIAN_POINT ( 'NONE',  ( -1.500000000000000222, -13.00000000000000533, -1.750000000000000000 ) ) ;
#6228 = ADVANCED_FACE ( 'NONE', ( #6340 ), #8681, .F. ) ;
#6229 = CIRCLE ( 'NONE', #492, 1.599999999999998979 ) ;
#6230 = DIRECTION ( 'NONE',  ( 0.000000000000000000, 0.000000000000000000, 1.000000000000000000 ) ) ;
#6231 = ORIENTED_EDGE ( 'NONE', *, *, #6108, .T. ) ;
#6232 = LINE ( 'NONE', #8684, #8799 ) ;
#6233 = CARTESIAN_POINT ( 'NONE',  ( 5.999999999999999112, 26.99999999999999289, -14.00000000000000178 ) ) ;
#6234 = CARTESIAN_POINT ( 'NONE',  ( -0.8124729078102072011, 5.726445515403652209, 1.383948283277976365 ) ) ;
#6235 = ORIENTED_EDGE ( 'NONE', *, *, #748, .F. ) ;
#6236 = EDGE_CURVE ( 'NONE', #6113, #798, #592, .T. ) ;
#6237 = LINE ( 'NONE', #3657, #9852 ) ;
#6238 = AXIS2_PLACEMENT_3D ( 'NONE', #8191, #4149, #7229 ) ;
#6239 = CARTESIAN_POINT ( 'NONE',  ( 30.00000000000001066, -25.00000000000000000, -1.999999999999997780 ) ) ;
#6240 = DIRECTION ( 'NONE',  ( 1.000000000000000000, 0.000000000000000000, 0.000000000000000000 ) ) ;
#6241 = AXIS2_PLACEMENT_3D ( 'NONE', #4284, #318, #9975 ) ;
#6242 = DIRECTION ( 'NONE',  ( 0.3420201433256627732, 0.9396926207859105373, 0.000000000000000000 ) ) ;
#6243 = DIRECTION ( 'NONE',  ( -1.000000000000000000, -0.000000000000000000, 0.000000000000000000 ) ) ;
#6244 = PLANE ( 'NONE',  #9080 ) ;
#6245 = CARTESIAN_POINT ( 'NONE',  ( 1.300000000000000044, 0.7390083445627224634, 1.279999999999999138 ) ) ;
#6246 = VECTOR ( 'NONE', #4978, 1000.000000000000000 ) ;
#6247 = CARTESIAN_POINT ( 'NONE',  ( 0.000000000000000000, 6.000000000000000000, -12.00000000000000000 ) ) ;
#6248 = CARTESIAN_POINT ( 'NONE',  ( -4.215868657802586128, -2.148092372876348133, 9.939999999999994174 ) ) ;
#6249 = STYLED_ITEM ( 'NONE', ( #982 ), #4712 ) ;
#6250 = CARTESIAN_POINT ( 'NONE',  ( -1.229367062500000163, -13.00000000000000533, -1.593750000682796708 ) ) ;
#6251 = CARTESIAN_POINT ( 'NONE',  ( -5.195105386651219348, -2.542276634908102295, 6.143948283277977040 ) ) ;
#6252 = EDGE_CURVE ( 'NONE', #2034, #8221, #676, .T. ) ;
#6253 = DIRECTION ( 'NONE',  ( -1.000000000000000000, -0.000000000000000000, -0.000000000000000000 ) ) ;
#6254 = CIRCLE ( 'NONE', #7457, 3.000000000000000000 ) ;
#6255 = VERTEX_POINT ( 'NONE', #6227 ) ;
#6256 = VECTOR ( 'NONE', #8768, 1000.000000000000000 ) ;
#6257 = CARTESIAN_POINT ( 'NONE',  ( 0.000000000000000000, -10.00000000000000000, -12.00000000000000000 ) ) ;
#6258 = PLANE ( 'NONE',  #6951 ) ;
#6259 = FACE_OUTER_BOUND ( 'NONE', #5337, .T. ) ;
#6260 = DIRECTION ( 'NONE',  ( 0.000000000000000000, 0.000000000000000000, 1.000000000000000000 ) ) ;
#6261 = ORIENTED_EDGE ( 'NONE', *, *, #10079, .T. ) ;
#6262 = CIRCLE ( 'NONE', #7978, 1.249999999999993339 ) ;
#6263 = CARTESIAN_POINT ( 'NONE',  ( 25.00000000000000000, 0.000000000000000000, -12.00000000000000000 ) ) ;
#6264 = CARTESIAN_POINT ( 'NONE',  ( -1.500000000000000222, -13.00000000000000533, -0.8125000013655935271 ) ) ;
#6265 = CARTESIAN_POINT ( 'NONE',  ( -2.042957248827969252, 4.009529358847651714, 10.63999999999999879 ) ) ;
#6266 = AXIS2_PLACEMENT_3D ( 'NONE', #4289, #3399, #2658 ) ;
#6267 = CARTESIAN_POINT ( 'NONE',  ( 0.7499999999999991118, -14.29903810567666333, -2.583333333333333481 ) ) ;
#6268 = CLOSED_SHELL ( 'NONE', ( #2596, #3716, #1023, #4349 ) ) ;
#6269 = ORIENTED_EDGE ( 'NONE', *, *, #4468, .F. ) ;
#6270 = VECTOR ( 'NONE', #2878, 1000.000000000000000 ) ;
#6271 = AXIS2_PLACEMENT_3D ( 'NONE', #2509, #4336, #6473 ) ;
#6272 = ORIENTED_EDGE ( 'NONE', *, *, #1753, .T. ) ;
#6273 = DIRECTION ( 'NONE',  ( -1.000000000000000000, -0.000000000000000000, -0.000000000000000000 ) ) ;
#6274 = EDGE_CURVE ( 'NONE', #3161, #118, #1790, .T. ) ;
#6275 = SURFACE_STYLE_USAGE ( .BOTH. , #5587 ) ;
#6276 = ORIENTED_EDGE ( 'NONE', *, *, #3517, .F. ) ;
#6277 = CARTESIAN_POINT ( 'NONE',  ( 5.418398423912711870, 0.9480714621563913758, 9.676051716722021467 ) ) ;
#6278 = CARTESIAN_POINT ( 'NONE',  ( 1.229367062500000163, -13.70977540446723886, 0.1145833326505366068 ) ) ;
#6279 = CARTESIAN_POINT ( 'NONE',  ( 10.00000000000000000, -7.851777359433979697, -3.255701506262516087 ) ) ;
#6280 = ORIENTED_EDGE ( 'NONE', *, *, #1197, .F. ) ;
#6281 = DIRECTION ( 'NONE',  ( -1.000000000000000000, -0.000000000000000000, -0.000000000000000000 ) ) ;
#6282 = CARTESIAN_POINT ( 'NONE',  ( 4.155232146225751322, -4.023224611898307934, 12.89605171672202211 ) ) ;
#6283 = VERTEX_POINT ( 'NONE', #5441 ) ;
#6284 = EDGE_CURVE ( 'NONE', #5844, #2608, #7080, .T. ) ;
#6285 = CARTESIAN_POINT ( 'NONE',  ( 1.500000000000000222, -13.00000000000000533, -0.06250000136559345776 ) ) ;
#6286 = EDGE_CURVE ( 'NONE', #4950, #5295, #7135, .T. ) ;
#6287 = FACE_OUTER_BOUND ( 'NONE', #3367, .T. ) ;
#6288 = EDGE_LOOP ( 'NONE', ( #2329, #5689, #10449, #1249 ) ) ;
#6289 = DIRECTION ( 'NONE',  ( 0.000000000000000000, -1.734723475976807094E-15, -1.000000000000000000 ) ) ;
#6290 = CARTESIAN_POINT ( 'NONE',  ( 0.9480714621563713917, 5.418398423912717199, 1.523948283277976268 ) ) ;
#6291 = VERTEX_POINT ( 'NONE', #4694 ) ;
#6292 = CARTESIAN_POINT ( 'NONE',  ( -1.500000000000000666, -13.86602540378444459, -1.770833334698926897 ) ) ;
#6293 = DIRECTION ( 'NONE',  ( 0.000000000000000000, 0.000000000000000000, -1.000000000000000000 ) ) ;
#6294 = ORIENTED_EDGE ( 'NONE', *, *, #5191, .T. ) ;
#6295 = EDGE_CURVE ( 'NONE', #2738, #980, #8719, .T. ) ;
#6296 = DIRECTION ( 'NONE',  ( -5.694029147589358720E-15, -6.585044023479645679E-31, 1.000000000000000000 ) ) ;
#6297 = DIRECTION ( 'NONE',  ( 0.3420201433256627732, -0.9396926207859105373, 0.000000000000000000 ) ) ;
#6298 = DIRECTION ( 'NONE',  ( -1.000000000000000000, -4.625929269271485914E-16, 0.000000000000000000 ) ) ;
#6299 = CARTESIAN_POINT ( 'NONE',  ( 4.000000000000000888, -7.851777359434023218, 3.255701506262409506 ) ) ;
#6300 = VECTOR ( 'NONE', #5298, 1000.000000000000000 ) ;
#6301 = LINE ( 'NONE', #8648, #6729 ) ;
#6302 = CARTESIAN_POINT ( 'NONE',  ( -0.7039550926810301812, -4.444597532678121965, 9.519999999999999574 ) ) ;
#6303 = CARTESIAN_POINT ( 'NONE',  ( 1.229367062499999719, -13.70977540446724063, -1.885416667349463449 ) ) ;
#6304 = CARTESIAN_POINT ( 'NONE',  ( 4.023224611898322145, -4.155232146225737111, 8.103948283277974340 ) ) ;
#6305 = FACE_OUTER_BOUND ( 'NONE', #3326, .T. ) ;
#6306 = VERTEX_POINT ( 'NONE', #10335 ) ;
#6307 = AXIS2_PLACEMENT_3D ( 'NONE', #2612, #7487, #228 ) ;
#6308 = CARTESIAN_POINT ( 'NONE',  ( -2.000000000000000000, 6.745408891279613961, -5.171987904998036178 ) ) ;
#6309 = CARTESIAN_POINT ( 'NONE',  ( 5.999999999999999112, -27.00000000000000711, -14.00000000000000178 ) ) ;
#6310 = ORIENTED_EDGE ( 'NONE', *, *, #10446, .T. ) ;
#6311 = DIRECTION ( 'NONE',  ( -0.000000000000000000, 1.000000000000000000, 0.000000000000000000 ) ) ;
#6312 = FACE_OUTER_BOUND ( 'NONE', #9774, .T. ) ;
#6313 = ORIENTED_EDGE ( 'NONE', *, *, #470, .T. ) ;
#6314 = CARTESIAN_POINT ( 'NONE',  ( 1.500000000000000222, -13.00000000000000533, -0.5625000013655934161 ) ) ;
#6315 = DIRECTION ( 'NONE',  ( -1.000000000000000000, -0.000000000000000000, -0.000000000000000000 ) ) ;
#6316 = MECHANICAL_DESIGN_GEOMETRIC_PRESENTATION_REPRESENTATION (  '', ( #7352 ), #2947 ) ;
#6317 = CARTESIAN_POINT ( 'NONE',  ( -3.345732310141667831, 3.345732310141653620, 10.50000000000000000 ) ) ;
#6318 = UNCERTAINTY_MEASURE_WITH_UNIT (LENGTH_MEASURE( 1.000000000000000082E-05 ), #3624, 'distance_accuracy_value', 'NONE');
#6319 = CARTESIAN_POINT ( 'NONE',  ( 1.500000000000000000, -13.86602540378444459, -1.041666666666666741 ) ) ;
#6320 = ORIENTED_EDGE ( 'NONE', *, *, #2718, .T. ) ;
#6321 = ADVANCED_FACE ( 'NONE', ( #569 ), #7191, .T. ) ;
#6322 = ORIENTED_EDGE ( 'NONE', *, *, #3507, .F. ) ;
#6323 = CIRCLE ( 'NONE', #10415, 1.249999999999988898 ) ;
#6324 = DIRECTION ( 'NONE',  ( -0.000000000000000000, -0.000000000000000000, -1.000000000000000000 ) ) ;
#6325 = CARTESIAN_POINT ( 'NONE',  ( 6.727620669667255804, 3.750000000000000000, -12.00000000000000000 ) ) ;
#6326 = EDGE_CURVE ( 'NONE', #9821, #9979, #7245, .T. ) ;
#6327 = ORIENTED_EDGE ( 'NONE', *, *, #4751, .T. ) ;
#6328 = CARTESIAN_POINT ( 'NONE',  ( -3.826313983664925811, -3.951860609387098489, 5.196051716722022817 ) ) ;
#6329 = CARTESIAN_POINT ( 'NONE',  ( 8.980342580332745683, -7.750000000000000000, 0.000000000000000000 ) ) ;
#6330 = FACE_OUTER_BOUND ( 'NONE', #4054, .T. ) ;
#6331 = ORIENTED_EDGE ( 'NONE', *, *, #3437, .F. ) ;
#6332 = CARTESIAN_POINT ( 'NONE',  ( 15.00000000000000000, 19.99999999999999645, 9.000000000000000000 ) ) ;
#6333 = CARTESIAN_POINT ( 'NONE',  ( 3.411736077305382420, -3.279728542977940364, 1.696051716722023484 ) ) ;
#6334 = EDGE_CURVE ( 'NONE', #4307, #9203, #8786, .T. ) ;
#6335 = VERTEX_POINT ( 'NONE', #9705 ) ;
#6336 =( NAMED_UNIT ( * ) SI_UNIT ( $, .STERADIAN. ) SOLID_ANGLE_UNIT ( ) );
#6337 = AXIS2_PLACEMENT_3D ( 'NONE', #7208, #8854, #5661 ) ;
#6338 = APPLICATION_CONTEXT ( 'automotive_design' ) ;
#6339 = VERTEX_POINT ( 'NONE', #5651 ) ;
#6340 = FACE_OUTER_BOUND ( 'NONE', #833, .T. ) ;
#6341 = PRODUCT_DEFINITION_FORMATION_WITH_SPECIFIED_SOURCE ( 'ANY', '', #5453, .NOT_KNOWN. ) ;
#6342 = CARTESIAN_POINT ( 'NONE',  ( 22.43558391966725907, -7.750000000000000000, -12.00000000000000000 ) ) ;
#6343 = ORIENTED_EDGE ( 'NONE', *, *, #4934, .T. ) ;
#6344 = DIRECTION ( 'NONE',  ( 1.000000000000000000, 0.000000000000000000, 0.000000000000000000 ) ) ;
#6345 = CARTESIAN_POINT ( 'NONE',  ( 10.69739119071655686, -10.02539999999999942, 0.000000000000000000 ) ) ;
#6346 = CARTESIAN_POINT ( 'NONE',  ( -3.951860609387083834, -3.826313983664940466, 6.003948283277975584 ) ) ;
#6347 = ORIENTED_EDGE ( 'NONE', *, *, #10055, .F. ) ;
#6348 = CIRCLE ( 'NONE', #8560, 0.1000000000000000472 ) ;
#6349 = CARTESIAN_POINT ( 'NONE',  ( -3.181725716174720498E-16, -14.73205080756888385, 0.3124999986344064729 ) ) ;
#6350 = EDGE_CURVE ( 'NONE', #346, #8266, #7356, .T. ) ;
#6351 = EDGE_CURVE ( 'NONE', #252, #7070, #2587, .T. ) ;
#6352 = DIRECTION ( 'NONE',  ( 0.000000000000000000, 0.000000000000000000, 1.000000000000000000 ) ) ;
#6353 = DIRECTION ( 'NONE',  ( 0.000000000000000000, 1.421085471520200372E-14, -1.000000000000000000 ) ) ;
#6354 = ORIENTED_EDGE ( 'NONE', *, *, #6223, .F. ) ;
#6355 = DIRECTION ( 'NONE',  ( -1.000000000000000000, 0.000000000000000000, 0.000000000000000000 ) ) ;
#6356 = AXIS2_PLACEMENT_3D ( 'NONE', #9028, #1764, #1922 ) ;
#6357 = LINE ( 'NONE', #2283, #2554 ) ;
#6358 = DIRECTION ( 'NONE',  ( -1.000000000000000000, 0.000000000000000000, 0.000000000000000000 ) ) ;
#6359 = DIRECTION ( 'NONE',  ( -1.000000000000000000, 0.000000000000000000, 0.000000000000000000 ) ) ;
#6360 = CARTESIAN_POINT ( 'NONE',  ( 1.300000000000000044, 0.000000000000000000, 1.280000000000000027 ) ) ;
#6361 = CARTESIAN_POINT ( 'NONE',  ( -4.673326407553653361, 0.7401821875142517992, 10.21999999999999709 ) ) ;
#6362 = CARTESIAN_POINT ( 'NONE',  ( -1.229367062500000163, -12.29022459553277002, -0.1354166673494631989 ) ) ;
#6363 = EDGE_CURVE ( 'NONE', #4105, #5643, #6348, .T. ) ;
#6364 = CARTESIAN_POINT ( 'NONE',  ( 5.432285873273257515, 0.8603895577212793411, 0.2799999999999999156 ) ) ;
#6365 = CARTESIAN_POINT ( 'NONE',  ( 0.000000000000000000, 0.000000000000000000, -9.000000000000000000 ) ) ;
#6366 = ORIENTED_EDGE ( 'NONE', *, *, #5072, .T. ) ;
#6367 = APPLICATION_PROTOCOL_DEFINITION ( 'draft international standard', 'automotive_design', 1998, #2562 ) ;
#6368 = LINE ( 'NONE', #71, #5422 ) ;
#6369 = DIRECTION ( 'NONE',  ( 0.000000000000000000, 0.000000000000000000, -1.000000000000000000 ) ) ;
#6370 = ORIENTED_EDGE ( 'NONE', *, *, #9355, .T. ) ;
#6371 = EDGE_CURVE ( 'NONE', #4487, #5555, #8161, .T. ) ;
#6372 = FACE_OUTER_BOUND ( 'NONE', #9438, .T. ) ;
#6373 = CARTESIAN_POINT ( 'NONE',  ( 8.000000000000001776, 0.000000000000000000, 0.000000000000000000 ) ) ;
#6374 = CARTESIAN_POINT ( 'NONE',  ( 9.980802115791359341, -13.63271488424911837, 0.000000000000000000 ) ) ;
#6375 = DIRECTION ( 'NONE',  ( 0.000000000000000000, 0.000000000000000000, 1.000000000000000000 ) ) ;
#6376 = LINE ( 'NONE', #3254, #5252 ) ;
#6377 = EDGE_CURVE ( 'NONE', #8600, #8955, #3374, .T. ) ;
#6378 = CARTESIAN_POINT ( 'NONE',  ( -4.444597532678119300, -0.7039550926810477227, 10.07999999999999829 ) ) ;
#6379 = CARTESIAN_POINT ( 'NONE',  ( 0.7499999999999991118, -14.29903810567666333, -2.083333333333333481 ) ) ;
#6380 = ORIENTED_EDGE ( 'NONE', *, *, #10438, .F. ) ;
#6381 = VERTEX_POINT ( 'NONE', #1842 ) ;
#6382 = DIRECTION ( 'NONE',  ( -1.000000000000000000, -0.000000000000000000, -0.000000000000000000 ) ) ;
#6383 = ORIENTED_EDGE ( 'NONE', *, *, #1658, .F. ) ;
#6384 = LINE ( 'NONE', #8046, #2018 ) ;
#6385 = DIRECTION ( 'NONE',  ( 0.000000000000000000, 0.000000000000000000, -1.000000000000000000 ) ) ;
#6386 = ORIENTED_EDGE ( 'NONE', *, *, #9268, .F. ) ;
#6387 = CARTESIAN_POINT ( 'NONE',  ( 20.11292429676619520, 6.000000000000000000, -12.00000000000000000 ) ) ;
#6388 = CARTESIAN_POINT ( 'NONE',  ( -0.8323763977770610722, 4.658724279160015413, 3.376051716722022977 ) ) ;
#6389 = ORIENTED_EDGE ( 'NONE', *, *, #10242, .T. ) ;
#6390 = ORIENTED_EDGE ( 'NONE', *, *, #3547, .T. ) ;
#6391 = CARTESIAN_POINT ( 'NONE',  ( 5.010572059283444624, -10.02539999999999942, -12.00000000000000000 ) ) ;
#6392 = DIRECTION ( 'NONE',  ( 0.3420201433256627732, -0.9396926207859105373, 0.000000000000000000 ) ) ;
#6393 = ORIENTED_EDGE ( 'NONE', *, *, #1152, .F. ) ;
#6394 = CARTESIAN_POINT ( 'NONE',  ( -5.432285873273256627, -0.8603895577212797852, 7.279999999999999361 ) ) ;
#6395 = EDGE_CURVE ( 'NONE', #4407, #138, #4267, .T. ) ;
#6396 = CARTESIAN_POINT ( 'NONE',  ( 3.000000000000002665, 0.000000000000000000, 0.000000000000000000 ) ) ;
#6397 = CARTESIAN_POINT ( 'NONE',  ( 5.195105386651219348, 2.542276634908100075, 4.743948283277974909 ) ) ;
#6398 = VERTEX_POINT ( 'NONE', #2484 ) ;
#6399 = CARTESIAN_POINT ( 'NONE',  ( -1.500000000000000666, -13.86602540378444459, -1.270833334698926897 ) ) ;
#6400 = ORIENTED_EDGE ( 'NONE', *, *, #9146, .T. ) ;
#6401 = CARTESIAN_POINT ( 'NONE',  ( 0.000000000000000000, -10.00000000000000000, -12.00000000000000000 ) ) ;
#6402 = CARTESIAN_POINT ( 'NONE',  ( 0.000000000000000000, 52.93638525830372998, 8.843061888689529582 ) ) ;
#6403 = FACE_BOUND ( 'NONE', #4910, .T. ) ;
#6404 = CARTESIAN_POINT ( 'NONE',  ( 5.999999999999999112, -27.00000000000000711, -14.00000000000000178 ) ) ;
#6405 = ADVANCED_FACE ( 'NONE', ( #1792 ), #3275, .T. ) ;
#6406 = CARTESIAN_POINT ( 'NONE',  ( 1.300000000000000044, 1.478016689125442484, -1.626303258728256651E-15 ) ) ;
#6407 = CARTESIAN_POINT ( 'NONE',  ( -3.345732310141667831, 3.345732310141653620, 7.699999999999998401 ) ) ;
#6408 = ORIENTED_EDGE ( 'NONE', *, *, #8711, .F. ) ;
#6409 = VECTOR ( 'NONE', #10384, 1000.000000000000000 ) ;
#6410 = CARTESIAN_POINT ( 'NONE',  ( 1.229367062500000163, -13.00000000000000533, -0.8437500006827965970 ) ) ;
#6411 = AXIS2_PLACEMENT_3D ( 'NONE', #2549, #2394, #5767 ) ;
#6412 = CARTESIAN_POINT ( 'NONE',  ( -5.697241258616385196, 0.9968613283357647958, 6.423948283277978177 ) ) ;
#6413 = LINE ( 'NONE', #9671, #7680 ) ;
#6414 = ORIENTED_EDGE ( 'NONE', *, *, #9804, .T. ) ;
#6415 = LINE ( 'NONE', #645, #8712 ) ;
#6416 = CARTESIAN_POINT ( 'NONE',  ( 1.999999999999975797, 15.00000000000000355, -6.000000000000009770 ) ) ;
#6417 = EDGE_CURVE ( 'NONE', #2194, #5388, #7713, .T. ) ;
#6418 = ORIENTED_EDGE ( 'NONE', *, *, #10438, .T. ) ;
#6419 = CARTESIAN_POINT ( 'NONE',  ( 8.161409553233806236, 6.000000000000000000, -12.00000000000000000 ) ) ;
#6420 = EDGE_CURVE ( 'NONE', #6225, #9635, #7405, .T. ) ;
#6421 = CARTESIAN_POINT ( 'NONE',  ( 1.500000000000000222, -13.00000000000000533, -1.500000000000000000 ) ) ;
#6422 = DIRECTION ( 'NONE',  ( 1.000000000000000000, 0.000000000000000000, 0.000000000000000000 ) ) ;
#6423 = CARTESIAN_POINT ( 'NONE',  ( 10.00000000000000000, -4.147285340411748678, -5.698247474649444477 ) ) ;
#6424 = DIRECTION ( 'NONE',  ( -1.000000000000000000, -0.000000000000000000, -0.000000000000000000 ) ) ;
#6425 = AXIS2_PLACEMENT_3D ( 'NONE', #3595, #6821, #6072 ) ;
#6426 = CARTESIAN_POINT ( 'NONE',  ( 4.258245684917310037, 2.064922774268912686, -0.8560517167220232926 ) ) ;
#6427 = UNCERTAINTY_MEASURE_WITH_UNIT (LENGTH_MEASURE( 1.000000000000000082E-05 ), #1683, 'distance_accuracy_value', 'NONE');
#6428 = AXIS2_PLACEMENT_3D ( 'NONE', #934, #5691, #9747 ) ;
#6429 = CARTESIAN_POINT ( 'NONE',  ( -1.500000000000000222, -13.00000000000000533, -0.2500000000000002220 ) ) ;
#6430 = ORIENTED_EDGE ( 'NONE', *, *, #2220, .F. ) ;
#6431 = ORIENTED_EDGE ( 'NONE', *, *, #1223, .T. ) ;
#6432 = EDGE_CURVE ( 'NONE', #9635, #8892, #774, .T. ) ;
#6433 = LINE ( 'NONE', #9696, #4411 ) ;
#6434 = CIRCLE ( 'NONE', #5249, 3.000000000000000000 ) ;
#6435 = DIRECTION ( 'NONE',  ( 1.000000000000000000, 1.156482317317871478E-16, 5.637851296924623057E-15 ) ) ;
#6436 = ORIENTED_EDGE ( 'NONE', *, *, #2136, .T. ) ;
#6437 = VECTOR ( 'NONE', #3772, 1000.000000000000000 ) ;
#6438 = CARTESIAN_POINT ( 'NONE',  ( 4.215868657802586128, 2.148092372876346801, 0.1400000000000000411 ) ) ;
#6439 = VECTOR ( 'NONE', #6134, 1000.000000000000000 ) ;
#6440 = VERTEX_POINT ( 'NONE', #146 ) ;
#6441 =( BOUNDED_CURVE ( )  B_SPLINE_CURVE ( 2, ( #849, #2334, #2282, #5505, #8693, #1544, #7148 ),
 .UNSPECIFIED., .F., .T. ) 
 B_SPLINE_CURVE_WITH_KNOTS ( ( 3, 2, 2, 3 ),
 ( 0.5833333333333332593, 0.6111111111111110494, 0.6388888888888888395, 0.6666666666666666297 ),
 .UNSPECIFIED. ) 
 CURVE ( )  GEOMETRIC_REPRESENTATION_ITEM ( )  RATIONAL_B_SPLINE_CURVE ( ( 1.000000000000000444, 0.8660254037844381525, 1.000000000000000000, 0.8660254037844387076, 1.000000000000000000, 0.8660254037844387076, 1.000000000000000000 ) ) 
 REPRESENTATION_ITEM ( '' )  );
#6442 = CARTESIAN_POINT ( 'NONE',  ( 4.940838830814703542, -2.417848759854246410, 12.75605171672202331 ) ) ;
#6443 = CIRCLE ( 'NONE', #8148, 1.999999999999997780 ) ;
#6444 = ORIENTED_EDGE ( 'NONE', *, *, #6196, .F. ) ;
#6445 = EDGE_LOOP ( 'NONE', ( #1578, #3059 ) ) ;
#6446 = AXIS2_PLACEMENT_3D ( 'NONE', #1581, #6281, #9537 ) ;
#6447 = DIRECTION ( 'NONE',  ( 0.3420201433256627732, -0.9396926207859105373, 0.000000000000000000 ) ) ;
#6448 = CARTESIAN_POINT ( 'NONE',  ( 4.414205890716556446, -10.02539999999999942, -12.00000000000000000 ) ) ;
#6449 = CIRCLE ( 'NONE', #6103, 2.500000000000000000 ) ;
#6450 = ORIENTED_EDGE ( 'NONE', *, *, #5143, .T. ) ;
#6451 = CARTESIAN_POINT ( 'NONE',  ( 5.432285873273257515, 0.8603895577212793411, 3.079999999999999627 ) ) ;
#6452 = DIRECTION ( 'NONE',  ( 0.000000000000000000, 0.000000000000000000, 1.000000000000000000 ) ) ;
#6453 = CARTESIAN_POINT ( 'NONE',  ( -4.023224611898323033, 4.155232146225737111, 9.503948283277974696 ) ) ;
#6454 = ORIENTED_EDGE ( 'NONE', *, *, #2609, .F. ) ;
#6455 = CARTESIAN_POINT ( 'NONE',  ( 0.7499999999999991118, -14.29903810567666333, -1.145833334698926897 ) ) ;
#6456 =( NAMED_UNIT ( * ) PLANE_ANGLE_UNIT ( ) SI_UNIT ( $, .RADIAN. ) );
#6457 = VERTEX_POINT ( 'NONE', #9106 ) ;
#6458 = DIRECTION ( 'NONE',  ( 0.000000000000000000, 0.000000000000000000, 1.000000000000000000 ) ) ;
#6459 = LINE ( 'NONE', #5765, #5427 ) ;
#6460 = CARTESIAN_POINT ( 'NONE',  ( 25.00000000000000000, -4.000000000000000000, -2.000000000000000000 ) ) ;
#6461 = DIRECTION ( 'NONE',  ( -1.000000000000000000, -0.000000000000000000, -0.000000000000000000 ) ) ;
#6462 = PLANE ( 'NONE',  #8954 ) ;
#6463 = CARTESIAN_POINT ( 'NONE',  ( -0.7401821875142701179, 4.673326407553649808, 13.57999999999999474 ) ) ;
#6464 = ORIENTED_EDGE ( 'NONE', *, *, #3901, .T. ) ;
#6465 = CARTESIAN_POINT ( 'NONE',  ( 1.999999999999975797, 15.00000000000000355, 6.000000000000010658 ) ) ;
#6466 = CARTESIAN_POINT ( 'NONE',  ( -0.9046671180729963790, 5.711843387010016926, 2.379999999999999893 ) ) ;
#6467 = LINE ( 'NONE', #5718, #5970 ) ;
#6468 = EDGE_CURVE ( 'NONE', #8145, #9102, #2532, .T. ) ;
#6469 = SHAPE_DEFINITION_REPRESENTATION ( #7058, #9732 ) ;
#6470 = CARTESIAN_POINT ( 'NONE',  ( 5.432285873273257515, 0.8603895577212793411, 0.2799999999999999156 ) ) ;
#6471 = DIRECTION ( 'NONE',  ( 1.000000000000000000, 2.312964634635742957E-16, -0.000000000000000000 ) ) ;
#6472 = CARTESIAN_POINT ( 'NONE',  ( 18.30309047890528618, -16.66178012940252273, 0.000000000000000000 ) ) ;
#6473 = DIRECTION ( 'NONE',  ( 0.000000000000000000, 0.000000000000000000, -1.000000000000000000 ) ) ;
#6474 = PRODUCT_DEFINITION_SHAPE ( 'NONE', 'NONE',  #496 ) ;
#6475 = FACE_OUTER_BOUND ( 'NONE', #1532, .T. ) ;
#6476 = DIRECTION ( 'NONE',  ( 1.000000000000000000, 0.000000000000000000, 0.000000000000000000 ) ) ;
#6477 = CARTESIAN_POINT ( 'NONE',  ( -31.74999999999995737, 0.000000000000000000, 1.500000000000000222 ) ) ;
#6478 = CARTESIAN_POINT ( 'NONE',  ( 0.7916369971161419938, 4.430710083317576320, 1.523948283277976268 ) ) ;
#6479 = CIRCLE ( 'NONE', #1921, 1.249999999999988898 ) ;
#6480 = EDGE_CURVE ( 'NONE', #118, #3946, #834, .T. ) ;
#6481 = CARTESIAN_POINT ( 'NONE',  ( -1.500000000000000000, -12.13397459621556607, -1.291666666666666963 ) ) ;
#6482 = EDGE_CURVE ( 'NONE', #4905, #2444, #8264, .T. ) ;
#6483 = ORIENTED_EDGE ( 'NONE', *, *, #5229, .T. ) ;
#6484 = ORIENTED_EDGE ( 'NONE', *, *, #10127, .T. ) ;
#6485 = DIRECTION ( 'NONE',  ( -0.000000000000000000, -0.000000000000000000, -1.000000000000000000 ) ) ;
#6486 = AXIS2_PLACEMENT_3D ( 'NONE', #4939, #4139, #6676 ) ;
#6487 = FACE_OUTER_BOUND ( 'NONE', #6288, .T. ) ;
#6488 = ORIENTED_EDGE ( 'NONE', *, *, #233, .T. ) ;
#6489 = CARTESIAN_POINT ( 'NONE',  ( -0.7039550926810301812, -4.444597532678121965, 3.919999999999999929 ) ) ;
#6490 = DIRECTION ( 'NONE',  ( 1.000000000000000000, 0.000000000000000000, -0.000000000000000000 ) ) ;
#6491 = ORIENTED_EDGE ( 'NONE', *, *, #6038, .F. ) ;
#6492 = CARTESIAN_POINT ( 'NONE',  ( 4.155232146225751322, -4.023224611898307934, 10.09605171672202140 ) ) ;
#6493 = EDGE_CURVE ( 'NONE', #9654, #2939, #6551, .T. ) ;
#6494 = EDGE_LOOP ( 'NONE', ( #3435, #5013, #9624, #3158 ) ) ;
#6495 = VECTOR ( 'NONE', #3604, 1000.000000000000000 ) ;
#6496 = CYLINDRICAL_SURFACE ( 'NONE', #4486, 6.248999999999999666 ) ;
#6497 = CARTESIAN_POINT ( 'NONE',  ( 1.500000000000000222, -12.13397459621556784, -1.958333333333333925 ) ) ;
#6498 = ORIENTED_EDGE ( 'NONE', *, *, #7065, .T. ) ;
#6499 = SHAPE_REPRESENTATION ( 'main housing', ( #2101 ), #4457 ) ;
#6500 = CARTESIAN_POINT ( 'NONE',  ( -5.152728359536494551, -2.625446233515535077, 1.540000000000000036 ) ) ;
#6501 = DIRECTION ( 'NONE',  ( -1.000000000000000000, -0.000000000000000000, -0.000000000000000000 ) ) ;
#6502 =( GEOMETRIC_REPRESENTATION_CONTEXT ( 3 ) GLOBAL_UNCERTAINTY_ASSIGNED_CONTEXT ( ( #7923 ) ) GLOBAL_UNIT_ASSIGNED_CONTEXT ( ( #6763, #7623, #3592 ) ) REPRESENTATION_CONTEXT ( 'NONE', 'WORKASPACE' ) );
#6503 = CARTESIAN_POINT ( 'NONE',  ( 5.432285873273257515, 0.8603895577212793411, 3.079999999999999627 ) ) ;
#6504 = ORIENTED_EDGE ( 'NONE', *, *, #8134, .F. ) ;
#6505 = CARTESIAN_POINT ( 'NONE',  ( 0.6146835312500001924, -11.93533689329915326, -2.635416667349463449 ) ) ;
#6506 = EDGE_CURVE ( 'NONE', #1459, #5116, #8392, .T. ) ;
#6507 = AXIS2_PLACEMENT_3D ( 'NONE', #5720, #10366, #7108 ) ;
#6508 = PRODUCT_DEFINITION_FORMATION_WITH_SPECIFIED_SOURCE ( 'ANY', '', #56, .NOT_KNOWN. ) ;
#6509 = ORIENTED_EDGE ( 'NONE', *, *, #9021, .T. ) ;
#6510 = CARTESIAN_POINT ( 'NONE',  ( 0.7499999999999991118, -14.29903810567666333, -2.583333333333333481 ) ) ;
#6511 = DIRECTION ( 'NONE',  ( -5.204170427930421283E-15, -6.018531076210112917E-31, -1.000000000000000000 ) ) ;
#6512 = CARTESIAN_POINT ( 'NONE',  ( 0.000000000000000000, -27.00000000000000711, 0.000000000000000000 ) ) ;
#6513 = DIRECTION ( 'NONE',  ( 0.000000000000000000, 0.000000000000000000, 1.000000000000000000 ) ) ;
#6514 = AXIS2_PLACEMENT_3D ( 'NONE', #6309, #1945, #5951 ) ;
#6515 = DIRECTION ( 'NONE',  ( -0.7043149233066458015, 0.7043149233066440251, -0.08877487040322762368 ) ) ;
#6516 = CARTESIAN_POINT ( 'NONE',  ( 4.458484982038663169, 0.6162731882459350219, 2.083948283277976543 ) ) ;
#6517 = ORIENTED_EDGE ( 'NONE', *, *, #5527, .F. ) ;
#6518 = CARTESIAN_POINT ( 'NONE',  ( 2.500000000000000000, 3.061616997868383141E-16, 3.000000000000000000 ) ) ;
#6519 = CARTESIAN_POINT ( 'NONE',  ( -0.8603895577212598011, -5.432285873273260179, 3.919999999999999929 ) ) ;
#6520 = PLANE ( 'NONE',  #7344 ) ;
#6521 = AXIS2_PLACEMENT_3D ( 'NONE', #305, #1998, #5217 ) ;
#6522 = ITEM_DEFINED_TRANSFORMATION ( 'NONE', 'NONE', #7020,  #2101 ) ;
#6523 = EDGE_CURVE ( 'NONE', #9213, #8065, #2637, .T. ) ;
#6524 = DIRECTION ( 'NONE',  ( -1.000000000000000000, 0.000000000000000000, -0.000000000000000000 ) ) ;
#6525 = AXIS2_PLACEMENT_3D ( 'NONE', #7056, #7004, #7226 ) ;
#6526 = FACE_OUTER_BOUND ( 'NONE', #10065, .T. ) ;
#6527 = DIRECTION ( 'NONE',  ( -0.3420201433256627732, -0.9396926207859105373, 0.000000000000000000 ) ) ;
#6528 = DIRECTION ( 'NONE',  ( 0.3420201433256627732, 0.9396926207859105373, -0.000000000000000000 ) ) ;
#6529 = ORIENTED_EDGE ( 'NONE', *, *, #8056, .F. ) ;
#6530 = CARTESIAN_POINT ( 'NONE',  ( -4.173491630687863108, -2.231261971483782691, 2.536051716722023119 ) ) ;
#6531 = TOROIDAL_SURFACE ( 'NONE', #1458, 2.600000000000000089, 0.1499999999999999944 ) ;
#6532 = ADVANCED_FACE ( 'NONE', ( #9001 ), #6496, .T. ) ;
#6533 = DIRECTION ( 'NONE',  ( -1.000000000000000000, 0.000000000000000000, 0.000000000000000000 ) ) ;
#6534 = DIRECTION ( 'NONE',  ( 1.000000000000000000, -0.000000000000000000, -0.000000000000000000 ) ) ;
#6535 = CIRCLE ( 'NONE', #4842, 3.000000000000000000 ) ;
#6536 = CARTESIAN_POINT ( 'NONE',  ( 3.969226411068985882, -2.122056237541205981, 5.163948283277975726 ) ) ;
#6537 = CARTESIAN_POINT ( 'NONE',  ( 1.530808498934180724E-16, -27.00000000000000711, 1.249999999999988898 ) ) ;
#6538 = VERTEX_POINT ( 'NONE', #9962 ) ;
#6539 = ORIENTED_EDGE ( 'NONE', *, *, #8887, .T. ) ;
#6540 = PLANE ( 'NONE',  #5933 ) ;
#6541 = DIRECTION ( 'NONE',  ( 0.000000000000000000, 0.000000000000000000, 1.000000000000000000 ) ) ;
#6542 = ORIENTED_EDGE ( 'NONE', *, *, #926, .T. ) ;
#6543 = CARTESIAN_POINT ( 'NONE',  ( 4.215868657802586128, 2.148092372876346801, 2.939999999999999503 ) ) ;
#6544 = CARTESIAN_POINT ( 'NONE',  ( 3.586028019667255595, -7.750000000000000000, -12.00000000000000000 ) ) ;
#6545 = ORIENTED_EDGE ( 'NONE', *, *, #1171, .F. ) ;
#6546 = CARTESIAN_POINT ( 'NONE',  ( 4.049832306626335310, -1.963858260114701215, 9.956051716722022604 ) ) ;
#6547 = PLANE ( 'NONE',  #558 ) ;
#6548 = EDGE_LOOP ( 'NONE', ( #9227, #667, #6444, #7685, #5340 ) ) ;
#6549 = SHAPE_REPRESENTATION_RELATIONSHIP ( 'NONE' , 'NONE' ,  #7954, #4603 ) ;
#6550 = ORIENTED_EDGE ( 'NONE', *, *, #1498, .F. ) ;
#6551 = LINE ( 'NONE', #9803, #6687 ) ;
#6552 = VERTEX_POINT ( 'NONE', #4964 ) ;
#6553 = ADVANCED_FACE ( 'NONE', ( #46 ), #9755, .F. ) ;
#6554 = CARTESIAN_POINT ( 'NONE',  ( 0.8603895577212593571, 5.432285873273261068, 2.519999999999999574 ) ) ;
#6555 = ADVANCED_FACE ( 'NONE', ( #8465 ), #9754, .T. ) ;
#6556 = CARTESIAN_POINT ( 'NONE',  ( 3.889087296526005488, 3.889087296526018811, 5.599999999999998757 ) ) ;
#6557 = CARTESIAN_POINT ( 'NONE',  ( 5.152728359536493663, 2.625446233515533745, 2.939999999999999059 ) ) ;
#6558 = ORIENTED_EDGE ( 'NONE', *, *, #712, .T. ) ;
#6559 = CARTESIAN_POINT ( 'NONE',  ( -0.6146835312499998594, -11.93533689329915326, -2.552083334016129967 ) ) ;
#6560 =( NAMED_UNIT ( * ) SI_UNIT ( $, .STERADIAN. ) SOLID_ANGLE_UNIT ( ) );
#6561 = ORIENTED_EDGE ( 'NONE', *, *, #1673, .F. ) ;
#6562 = PRODUCT_DEFINITION_SHAPE ( 'NONE', 'NONE',  #10504 ) ;
#6563 = FACE_OUTER_BOUND ( 'NONE', #5032, .T. ) ;
#6564 = LINE ( 'NONE', #5662, #3402 ) ;
#6565 = FACE_OUTER_BOUND ( 'NONE', #4155, .T. ) ;
#6566 = EDGE_CURVE ( 'NONE', #7403, #2210, #4317, .T. ) ;
#6567 = FACE_OUTER_BOUND ( 'NONE', #2841, .T. ) ;
#6568 = CARTESIAN_POINT ( 'NONE',  ( 0.6146835312500001924, -11.93533689329915326, -2.260416667349463449 ) ) ;
#6569 = CARTESIAN_POINT ( 'NONE',  ( -3.969226411068985882, 2.122056237541205537, 0.9639482832779766586 ) ) ;
#6570 = ORIENTED_EDGE ( 'NONE', *, *, #5996, .F. ) ;
#6571 = CARTESIAN_POINT ( 'NONE',  ( -1.229367062500000385, -13.70977540446723886, -0.05208333401612993269 ) ) ;
#6572 = CARTESIAN_POINT ( 'NONE',  ( 3.889087296526005488, 3.889087296526018811, 2.799999999999999378 ) ) ;
#6573 = CARTESIAN_POINT ( 'NONE',  ( 3.586028019667255595, -7.750000000000000000, -12.00000000000000000 ) ) ;
#6574 = CARTESIAN_POINT ( 'NONE',  ( -5.711843387010019590, 0.9046671180729746187, 10.21999999999999886 ) ) ;
#6575 = CYLINDRICAL_SURFACE ( 'NONE', #6356, 3.000000000000000000 ) ;
#6576 = CARTESIAN_POINT ( 'NONE',  ( 1.878224253233805818, 6.000000000000000000, -12.00000000000000000 ) ) ;
#6577 = VECTOR ( 'NONE', #4876, 1000.000000000000000 ) ;
#6578 = DIRECTION ( 'NONE',  ( 0.000000000000000000, 0.000000000000000000, 1.000000000000000000 ) ) ;
#6579 = CARTESIAN_POINT ( 'NONE',  ( 27.00000000000001066, 0.000000000000000000, -1.599999999999992983 ) ) ;
#6580 = CARTESIAN_POINT ( 'NONE',  ( -2.064922774268895811, -4.258245684917318918, 5.056051716722023137 ) ) ;
#6581 = CARTESIAN_POINT ( 'NONE',  ( 25.00000000000000000, -4.000000000000000000, -10.00000000000000000 ) ) ;
#6582 = CARTESIAN_POINT ( 'NONE',  ( -1.963858260114716980, 4.049832306626327316, 6.843948283277976330 ) ) ;
#6583 = DIRECTION ( 'NONE',  ( 0.000000000000000000, 0.000000000000000000, -1.000000000000000000 ) ) ;
#6584 = ORIENTED_EDGE ( 'NONE', *, *, #2859, .F. ) ;
#6585 = AXIS2_PLACEMENT_3D ( 'NONE', #5237, #8335, #422 ) ;
#6586 = CARTESIAN_POINT ( 'NONE',  ( 5.418398423912711870, 0.9480714621563913758, 4.076051716722022711 ) ) ;
#6587 = EDGE_LOOP ( 'NONE', ( #6984, #1879, #988, #6908 ) ) ;
#6588 = CARTESIAN_POINT ( 'NONE',  ( 15.26352788033274699, 3.750000000000000000, -12.00000000000000000 ) ) ;
#6589 = VECTOR ( 'NONE', #8243, 1000.000000000000000 ) ;
#6590 = DIRECTION ( 'NONE',  ( -1.000000000000000000, 0.000000000000000000, -0.000000000000000000 ) ) ;
#6591 = ORIENTED_EDGE ( 'NONE', *, *, #2418, .T. ) ;
#6592 = VECTOR ( 'NONE', #9596, 1000.000000000000000 ) ;
#6593 = DIRECTION ( 'NONE',  ( 0.000000000000000000, 0.000000000000000000, -1.000000000000000000 ) ) ;
#6594 = PLANE ( 'NONE',  #7783 ) ;
#6595 = EDGE_LOOP ( 'NONE', ( #6882, #820, #9700, #5640 ) ) ;
#6596 = COLOUR_RGB ( '', 0.40784314, 0.44705882, 0.49803922) ;
#6597 = CARTESIAN_POINT ( 'NONE',  ( 2.064922774268895811, 4.258245684917319807, 9.256051716722023315 ) ) ;
#6598 = CARTESIAN_POINT ( 'NONE',  ( -2.000000000000013767, 15.00000000000000355, -3.999999999999988898 ) ) ;
#6599 = ORIENTED_EDGE ( 'NONE', *, *, #2278, .T. ) ;
#6600 =( NAMED_UNIT ( * ) SI_UNIT ( $, .STERADIAN. ) SOLID_ANGLE_UNIT ( ) );
#6601 = AXIS2_PLACEMENT_3D ( 'NONE', #9260, #8571, #2000 ) ;
#6602 = ADVANCED_FACE ( 'NONE', ( #3877 ), #2050, .F. ) ;
#6603 = ORIENTED_EDGE ( 'NONE', *, *, #5598, .F. ) ;
#6604 = DIRECTION ( 'NONE',  ( -5.694029147589358720E-15, -6.585044023479645679E-31, 1.000000000000000000 ) ) ;
#6605 = CIRCLE ( 'NONE', #7624, 8.500000000000000000 ) ;
#6606 = ORIENTED_EDGE ( 'NONE', *, *, #3373, .T. ) ;
#6607 = CARTESIAN_POINT ( 'NONE',  ( -2.496947748567517333, 4.900535883036019058, 2.239999999999999769 ) ) ;
#6608 = CARTESIAN_POINT ( 'NONE',  ( 2.496947748567516889, -4.900535883036019946, 6.439999999999999503 ) ) ;
#6609 = CIRCLE ( 'NONE', #4759, 3.000000000000000888 ) ;
#6610 = CARTESIAN_POINT ( 'NONE',  ( -4.860232935257354114, 2.576046737280751842, 12.16394828327797661 ) ) ;
#6611 = VERTEX_POINT ( 'NONE', #7721 ) ;
#6612 = AXIS2_PLACEMENT_3D ( 'NONE', #8709, #548, #7057 ) ;
#6613 = CARTESIAN_POINT ( 'NONE',  ( 8.692241771943169307E-17, -11.58044919106553294, -2.093750000682796486 ) ) ;
#6614 = VECTOR ( 'NONE', #1163, 1000.000000000000000 ) ;
#6615 = EDGE_CURVE ( 'NONE', #4686, #10490, #5168, .T. ) ;
#6616 = EDGE_CURVE ( 'NONE', #4950, #2005, #8418, .T. ) ;
#6617 = ORIENTED_EDGE ( 'NONE', *, *, #845, .T. ) ;
#6618 = CIRCLE ( 'NONE', #8831, 1.600000000000000311 ) ;
#6619 = DIRECTION ( 'NONE',  ( 0.000000000000000000, 0.000000000000000000, 1.000000000000000000 ) ) ;
#6620 = CARTESIAN_POINT ( 'NONE',  ( 4.404961046766194599, -10.00000000000000000, 0.000000000000000000 ) ) ;
#6621 = DIRECTION ( 'NONE',  ( 0.000000000000000000, 0.000000000000000000, 1.000000000000000000 ) ) ;
#6622 = VERTEX_POINT ( 'NONE', #6114 ) ;
#6623 = LINE ( 'NONE', #1005, #2139 ) ;
#6624 = CARTESIAN_POINT ( 'NONE',  ( 1.229367062500000163, -12.29022459553277002, -1.302083334016129967 ) ) ;
#6625 = CARTESIAN_POINT ( 'NONE',  ( 3.345732310141667387, -3.345732310141653620, 11.90000000000000036 ) ) ;
#6626 = VERTEX_POINT ( 'NONE', #2245 ) ;
#6627 = LINE ( 'NONE', #10038, #5761 ) ;
#6628 = CARTESIAN_POINT ( 'NONE',  ( -5.711843387010018702, 0.9046671180729746187, 7.419999999999998153 ) ) ;
#6629 = ADVANCED_FACE ( 'NONE', ( #4475 ), #7612, .F. ) ;
#6630 = DIRECTION ( 'NONE',  ( -1.000000000000000000, -0.000000000000000000, -0.000000000000000000 ) ) ;
#6631 = CARTESIAN_POINT ( 'NONE',  ( -3.889087296526005044, -3.889087296526019255, 4.200000000000000178 ) ) ;
#6632 = LINE ( 'NONE', #2663, #781 ) ;
#6633 = FACE_OUTER_BOUND ( 'NONE', #8311, .T. ) ;
#6634 = DIRECTION ( 'NONE',  ( -0.3420201433256627732, -0.9396926207859105373, 0.000000000000000000 ) ) ;
#6635 = CARTESIAN_POINT ( 'NONE',  ( -4.430710083317573655, -0.7916369971161599794, 8.276051716722021112 ) ) ;
#6636 = FILL_AREA_STYLE ('',( #920 ) ) ;
#6637 = CARTESIAN_POINT ( 'NONE',  ( 2.231261971483764484, 4.173491630687871101, 7.263948283277976259 ) ) ;
#6638 = CARTESIAN_POINT ( 'NONE',  ( 27.00000000000001066, -25.00000000000000000, -1.999999999999997780 ) ) ;
#6639 = ORIENTED_EDGE ( 'NONE', *, *, #8845, .F. ) ;
#6640 = CARTESIAN_POINT ( 'NONE',  ( -2.576046737280769605, 4.860232935257343456, 3.236051716722023297 ) ) ;
#6641 = LINE ( 'NONE', #7444, #3243 ) ;
#6642 = CARTESIAN_POINT ( 'NONE',  ( -17.00000000000000000, 19.99999999999999645, -9.000000000000000000 ) ) ;
#6643 = ORIENTED_EDGE ( 'NONE', *, *, #10008, .T. ) ;
#6644 = CARTESIAN_POINT ( 'NONE',  ( 3.181980515339458471, 3.181980515339470461, 2.799999999999999378 ) ) ;
#6645 = VECTOR ( 'NONE', #7085, 1000.000000000000000 ) ;
#6646 = ORIENTED_EDGE ( 'NONE', *, *, #3043, .T. ) ;
#6647 = CARTESIAN_POINT ( 'NONE',  ( 4.687928535947288644, -0.6479879772514620662, 12.61605171672202097 ) ) ;
#6648 = CARTESIAN_POINT ( 'NONE',  ( -0.7500000000000007772, -14.29903810567666156, -1.229166668032260157 ) ) ;
#6649 = ORIENTED_EDGE ( 'NONE', *, *, #1901, .F. ) ;
#6650 = ORIENTED_EDGE ( 'NONE', *, *, #9736, .F. ) ;
#6651 = EDGE_CURVE ( 'NONE', #9748, #4597, #3089, .T. ) ;
#6652 = CARTESIAN_POINT ( 'NONE',  ( 0.000000000000000000, -13.00000000000000533, 0.000000000000000000 ) ) ;
#6653 = CARTESIAN_POINT ( 'NONE',  ( 1.500000000000000222, -13.00000000000000533, -0.5000000000000000000 ) ) ;
#6654 = ORIENTED_EDGE ( 'NONE', *, *, #5502, .F. ) ;
#6655 = CARTESIAN_POINT ( 'NONE',  ( -4.155232146225753098, 4.023224611898306158, 3.096051716722023617 ) ) ;
#6656 = CARTESIAN_POINT ( 'NONE',  ( 0.9046671180729951578, -5.711843387010016926, 6.579999999999999183 ) ) ;
#6657 = CARTESIAN_POINT ( 'NONE',  ( 2.708615832122949652, 5.110351332421781301, 10.06394828327797519 ) ) ;
#6658 = ORIENTED_EDGE ( 'NONE', *, *, #4936, .T. ) ;
#6659 = CARTESIAN_POINT ( 'NONE',  ( -2.607672531582950546E-16, -14.41955080893447416, -0.8437500006827965970 ) ) ;
#6660 = EDGE_CURVE ( 'NONE', #274, #2223, #415, .T. ) ;
#6661 = VECTOR ( 'NONE', #7901, 1000.000000000000000 ) ;
#6662 =( LENGTH_UNIT ( ) NAMED_UNIT ( * ) SI_UNIT ( .MILLI., .METRE. ) );
#6663 = ORIENTED_EDGE ( 'NONE', *, *, #7781, .T. ) ;
#6664 = DIRECTION ( 'NONE',  ( 0.000000000000000000, 1.000000000000000000, 0.000000000000000000 ) ) ;
#6665 = FACE_OUTER_BOUND ( 'NONE', #472, .T. ) ;
#6666 = CARTESIAN_POINT ( 'NONE',  ( -2.000000000000000000, -5.233522515400119701, 4.720195129223260899 ) ) ;
#6667 = ORIENTED_EDGE ( 'NONE', *, *, #1033, .T. ) ;
#6668 = AXIS2_PLACEMENT_3D ( 'NONE', #3016, #9274, #4439 ) ;
#6669 = CARTESIAN_POINT ( 'NONE',  ( 16.97133164676619899, -10.00000000000000178, 0.000000000000000000 ) ) ;
#6670 = CARTESIAN_POINT ( 'NONE',  ( -1.229367062500000163, -12.29022459553277002, -2.135416667349463449 ) ) ;
#6671 = CARTESIAN_POINT ( 'NONE',  ( -1.963858260114716980, 4.049832306626327316, 4.043948283277976508 ) ) ;
#6672 = ORIENTED_EDGE ( 'NONE', *, *, #10200, .T. ) ;
#6673 = DIRECTION ( 'NONE',  ( 0.000000000000000000, 0.000000000000000000, 1.000000000000000000 ) ) ;
#6674 = EDGE_CURVE ( 'NONE', #1096, #5848, #10013, .T. ) ;
#6675 = CARTESIAN_POINT ( 'NONE',  ( -5.432285873273256627, -0.8603895577212797852, 4.479999999999999538 ) ) ;
#6676 = DIRECTION ( 'NONE',  ( 0.000000000000000000, 0.000000000000000000, -1.000000000000000000 ) ) ;
#6677 = CARTESIAN_POINT ( 'NONE',  ( -0.9046671180729962680, 5.711843387010016926, 10.77999999999999936 ) ) ;
#6678 = AXIS2_PLACEMENT_3D ( 'NONE', #9778, #7971, #5521 ) ;
#6679 = LINE ( 'NONE', #9937, #5008 ) ;
#6680 = FACE_BOUND ( 'NONE', #4682, .T. ) ;
#6681 = MECHANICAL_DESIGN_GEOMETRIC_PRESENTATION_REPRESENTATION (  '', ( #2794 ), #9751 ) ;
#6682 = CARTESIAN_POINT ( 'NONE',  ( 0.000000000000000000, -10.00000000000000000, 0.000000000000000000 ) ) ;
#6683 = CARTESIAN_POINT ( 'NONE',  ( -0.8323763977770610722, 4.658724279160015413, 3.376051716722022977 ) ) ;
#6684 = EDGE_CURVE ( 'NONE', #3281, #6538, #8235, .T. ) ;
#6685 = EDGE_CURVE ( 'NONE', #6166, #1958, #601, .T. ) ;
#6686 = CARTESIAN_POINT ( 'NONE',  ( -2.607672531582950546E-16, -14.41955080893447416, -2.343750000682796930 ) ) ;
#6687 = VECTOR ( 'NONE', #1046, 1000.000000000000000 ) ;
#6688 = CARTESIAN_POINT ( 'NONE',  ( 4.658724279160018966, -0.8323763977770426425, 5.023948283277976046 ) ) ;
#6689 = CARTESIAN_POINT ( 'NONE',  ( -1.229367062500000163, -13.70977540446723708, -2.427083334016129967 ) ) ;
#6690 = VERTEX_POINT ( 'NONE', #3683 ) ;
#6691 = CARTESIAN_POINT ( 'NONE',  ( 5.110351332421769754, 2.708615832122969191, 3.936051716722023031 ) ) ;
#6692 = LINE ( 'NONE', #5007, #199 ) ;
#6693 = VECTOR ( 'NONE', #9832, 1000.000000000000000 ) ;
#6694 = DIRECTION ( 'NONE',  ( 0.000000000000000000, 0.5000000000000013323, 0.8660254037844378194 ) ) ;
#6695 = ORIENTED_EDGE ( 'NONE', *, *, #4468, .T. ) ;
#6696 = EDGE_CURVE ( 'NONE', #201, #4238, #5277, .T. ) ;
#6697 = AXIS2_PLACEMENT_3D ( 'NONE', #2924, #5304, #3559 ) ;
#6698 = CARTESIAN_POINT ( 'NONE',  ( -4.009529358847660596, 2.042957248827953265, 7.559999999999998721 ) ) ;
#6699 = CARTESIAN_POINT ( 'NONE',  ( 4.049832306626335310, -1.963858260114701215, 12.75605171672202331 ) ) ;
#6700 = CARTESIAN_POINT ( 'NONE',  ( 8.692241771943169307E-17, -11.58044919106553294, -2.218750000682796486 ) ) ;
#6701 = ORIENTED_EDGE ( 'NONE', *, *, #2389, .F. ) ;
#6702 = SURFACE_STYLE_USAGE ( .BOTH. , #4264 ) ;
#6703 = ORIENTED_EDGE ( 'NONE', *, *, #4812, .T. ) ;
#6704 = DIRECTION ( 'NONE',  ( 0.000000000000000000, 1.224646799147353207E-16, 1.000000000000000000 ) ) ;
#6705 = DIRECTION ( 'NONE',  ( 1.000000000000000000, 0.000000000000000000, 0.000000000000000000 ) ) ;
#6706 = ORIENTED_EDGE ( 'NONE', *, *, #9355, .F. ) ;
#6707 = CARTESIAN_POINT ( 'NONE',  ( 2.542276634908080535, 5.195105386651229118, 3.656051716722022782 ) ) ;
#6708 = CARTESIAN_POINT ( 'NONE',  ( -0.9046671180729963790, 5.711843387010016926, 2.379999999999999893 ) ) ;
#6709 = CARTESIAN_POINT ( 'NONE',  ( -2.496947748567517333, 4.900535883036019058, 10.63999999999999879 ) ) ;
#6710 = ORIENTED_EDGE ( 'NONE', *, *, #6887, .F. ) ;
#6711 = CARTESIAN_POINT ( 'NONE',  ( 0.6146835312500001924, -11.93533689329915326, -1.635416667349463227 ) ) ;
#6712 = ORIENTED_EDGE ( 'NONE', *, *, #6274, .T. ) ;
#6713 = CYLINDRICAL_SURFACE ( 'NONE', #3471, 3.000000000000000000 ) ;
#6714 = ORIENTED_EDGE ( 'NONE', *, *, #1809, .F. ) ;
#6715 = DIRECTION ( 'NONE',  ( -0.000000000000000000, -0.000000000000000000, 1.000000000000000000 ) ) ;
#6716 = CARTESIAN_POINT ( 'NONE',  ( -0.6146835312500006365, -14.06466310670085562, -1.010416667349463227 ) ) ;
#6717 = CARTESIAN_POINT ( 'NONE',  ( -2.231261971483764484, -4.173491630687871101, 11.46394828327797555 ) ) ;
#6718 = ORIENTED_EDGE ( 'NONE', *, *, #3649, .T. ) ;
#6719 = CARTESIAN_POINT ( 'NONE',  ( 13.83898384071655840, 6.025400000000000311, -12.00000000000000000 ) ) ;
#6720 = CARTESIAN_POINT ( 'NONE',  ( -0.8603895577212598011, -5.432285873273260179, 9.519999999999999574 ) ) ;
#6721 = DIRECTION ( 'NONE',  ( 1.000000000000000000, 0.000000000000000000, -0.000000000000000000 ) ) ;
#6722 = CARTESIAN_POINT ( 'NONE',  ( -5.432285873273256627, -0.8603895577212797852, 10.07999999999999829 ) ) ;
#6723 = EDGE_CURVE ( 'NONE', #8225, #5844, #1198, .T. ) ;
#6724 = FACE_OUTER_BOUND ( 'NONE', #7833, .T. ) ;
#6725 = CARTESIAN_POINT ( 'NONE',  ( 8.000000000000001776, 5.904264776415100613, 2.046865518294722630 ) ) ;
#6726 = CARTESIAN_POINT ( 'NONE',  ( 8.980342580332745683, 3.750000000000000000, -12.00000000000000000 ) ) ;
#6727 = CARTESIAN_POINT ( 'NONE',  ( -0.8323763977770610722, 4.658724279160015413, 8.976051716722020402 ) ) ;
#6728 = CARTESIAN_POINT ( 'NONE',  ( -0.6146835312499998594, -11.93533689329915326, -2.552083334016129967 ) ) ;
#6729 = VECTOR ( 'NONE', #2180, 1000.000000000000000 ) ;
#6730 = CARTESIAN_POINT ( 'NONE',  ( 2.708615832122949652, 5.110351332421781301, 1.663948283277976392 ) ) ;
#6731 = DIRECTION ( 'NONE',  ( 0.000000000000000000, 0.000000000000000000, 1.000000000000000000 ) ) ;
#6732 = EDGE_CURVE ( 'NONE', #2162, #9974, #5342, .T. ) ;
#6733 = ORIENTED_EDGE ( 'NONE', *, *, #10068, .F. ) ;
#6734 = EDGE_CURVE ( 'NONE', #8580, #7607, #8366, .T. ) ;
#6735 = CARTESIAN_POINT ( 'NONE',  ( -5.110351332421769754, -2.708615832122969191, 8.136051716722024096 ) ) ;
#6736 = ADVANCED_BREP_SHAPE_REPRESENTATION ( '', ( #8241, #2101 ), #9398 ) ;
#6737 = EDGE_CURVE ( 'NONE', #2034, #9654, #6860, .T. ) ;
#6738 = VECTOR ( 'NONE', #9333, 1000.000000000000000 ) ;
#6739 = CARTESIAN_POINT ( 'NONE',  ( -2.000000000000000000, 5.241389472434725860, -4.711457988287000909 ) ) ;
#6740 = DIRECTION ( 'NONE',  ( -0.000000000000000000, 1.000000000000000000, 0.000000000000000000 ) ) ;
#6741 = EDGE_LOOP ( 'NONE', ( #8710, #5066 ) ) ;
#6742 = CARTESIAN_POINT ( 'NONE',  ( -4.673326407553653361, 0.7401821875142517992, 10.21999999999999886 ) ) ;
#6743 = SURFACE_STYLE_FILL_AREA ( #1038 ) ;
#6744 = AXIS2_PLACEMENT_3D ( 'NONE', #28, #3304, #972 ) ;
#6745 = CARTESIAN_POINT ( 'NONE',  ( -4.687928535947287756, 0.6479879772514611780, 8.416051716722021681 ) ) ;
#6746 = AXIS2_PLACEMENT_3D ( 'NONE', #1701, #7259, #9874 ) ;
#6747 = CARTESIAN_POINT ( 'NONE',  ( 6.727620669667255804, -7.750000000000000000, -12.00000000000000000 ) ) ;
#6748 = ORIENTED_EDGE ( 'NONE', *, *, #227, .T. ) ;
#6749 = EDGE_CURVE ( 'NONE', #7985, #4115, #7885, .T. ) ;
#6750 = CIRCLE ( 'NONE', #3042, 3.000000000000000000 ) ;
#6751 = VERTEX_POINT ( 'NONE', #9728 ) ;
#6752 = CARTESIAN_POINT ( 'NONE',  ( 0.000000000000000000, -4.000000000000000000, -12.00000000000000000 ) ) ;
#6753 = VECTOR ( 'NONE', #5546, 1000.000000000000000 ) ;
#6754 = CARTESIAN_POINT ( 'NONE',  ( -26.99999999999998934, 0.000000000000000000, 0.000000000000000000 ) ) ;
#6755 = ORIENTED_EDGE ( 'NONE', *, *, #3199, .F. ) ;
#6756 = CIRCLE ( 'NONE', #9312, 2.000000000000000000 ) ;
#6757 = CARTESIAN_POINT ( 'NONE',  ( 2.576046737280769605, -4.860232935257343456, 4.636051716722022320 ) ) ;
#6758 = CARTESIAN_POINT ( 'NONE',  ( 4.900535883036028828, -2.496947748567499126, 0.5599999999999999423 ) ) ;
#6759 = CARTESIAN_POINT ( 'NONE',  ( -5.711843387010018702, 0.9046671180729746187, 13.01999999999999424 ) ) ;
#6760 = ORIENTED_EDGE ( 'NONE', *, *, #8400, .T. ) ;
#6761 = CARTESIAN_POINT ( 'NONE',  ( 0.6146835312499993043, -14.06466310670085562, -1.302083334016129967 ) ) ;
#6762 = AXIS2_PLACEMENT_3D ( 'NONE', #2840, #2053, #8520 ) ;
#6763 =( LENGTH_UNIT ( ) NAMED_UNIT ( * ) SI_UNIT ( .MILLI., .METRE. ) );
#6764 = VECTOR ( 'NONE', #6534, 1000.000000000000000 ) ;
#6765 = ORIENTED_EDGE ( 'NONE', *, *, #8426, .T. ) ;
#6766 = CARTESIAN_POINT ( 'NONE',  ( -29.99999999999998934, 0.000000000000000000, 0.000000000000000000 ) ) ;
#6767 = CARTESIAN_POINT ( 'NONE',  ( 14.43535000928344481, -10.02539999999999942, -12.00000000000000000 ) ) ;
#6768 = ORIENTED_EDGE ( 'NONE', *, *, #2937, .T. ) ;
#6769 = DIRECTION ( 'NONE',  ( -0.000000000000000000, -0.000000000000000000, 1.000000000000000000 ) ) ;
#6770 = AXIS2_PLACEMENT_3D ( 'NONE', #1290, #4357, #9196 ) ;
#6771 = CARTESIAN_POINT ( 'NONE',  ( 24.68830583033274806, 3.750000000000000000, 0.000000000000000000 ) ) ;
#6772 = CARTESIAN_POINT ( 'NONE',  ( -1.229367062500000163, -13.00000000000000533, -2.593750000682796486 ) ) ;
#6773 = CARTESIAN_POINT ( 'NONE',  ( -3.279728542977953687, 3.411736077305369541, 12.30394828327797718 ) ) ;
#6774 = ORIENTED_EDGE ( 'NONE', *, *, #4515, .T. ) ;
#6775 = CIRCLE ( 'NONE', #7292, 1.500000000000000222 ) ;
#6776 = DIRECTION ( 'NONE',  ( 1.156482317317871478E-16, -1.000000000000000000, -0.000000000000000000 ) ) ;
#6777 = AXIS2_PLACEMENT_3D ( 'NONE', #1009, #5037, #6673 ) ;
#6778 = EDGE_CURVE ( 'NONE', #8930, #1347, #5624, .T. ) ;
#6779 = CARTESIAN_POINT ( 'NONE',  ( 2.625446233515515537, 5.152728359536502545, 13.85999999999999766 ) ) ;
#6780 = VECTOR ( 'NONE', #5373, 1000.000000000000000 ) ;
#6781 = CARTESIAN_POINT ( 'NONE',  ( 4.000000000000000888, -5.848742439617878652, -6.167836887841048110 ) ) ;
#6782 = PRESENTATION_LAYER_ASSIGNMENT (  '', '', ( #9215 ) ) ;
#6783 = CARTESIAN_POINT ( 'NONE',  ( 3.889087296526005488, 3.889087296526018811, 5.599999999999998757 ) ) ;
#6784 = CIRCLE ( 'NONE', #6100, 8.500000000000000000 ) ;
#6785 = DIRECTION ( 'NONE',  ( 0.000000000000000000, 0.000000000000000000, 1.000000000000000000 ) ) ;
#6786 = EDGE_CURVE ( 'NONE', #8730, #2255, #8081, .T. ) ;
#6787 = DIRECTION ( 'NONE',  ( 1.000000000000000000, 0.000000000000000000, 0.000000000000000000 ) ) ;
#6788 = CARTESIAN_POINT ( 'NONE',  ( 2.697157280332745266, -7.750000000000000000, -12.00000000000000000 ) ) ;
#6789 = CARTESIAN_POINT ( 'NONE',  ( -0.8323763977770610722, 4.658724279160015413, 11.77605171672202289 ) ) ;
#6790 = CARTESIAN_POINT ( 'NONE',  ( 1.300000000000000044, -1.478016689125442706, 1.843143693225357538E-15 ) ) ;
#6791 = ADVANCED_FACE ( 'NONE', ( #6526 ), #1660, .T. ) ;
#6792 = CARTESIAN_POINT ( 'NONE',  ( -0.8124729078102072011, 5.726445515403652209, 1.383948283277976365 ) ) ;
#6793 = CARTESIAN_POINT ( 'NONE',  ( 8.692241771943170539E-17, -11.58044919106553650, -1.093750000682796486 ) ) ;
#6794 = ORIENTED_EDGE ( 'NONE', *, *, #1723, .F. ) ;
#6795 = CARTESIAN_POINT ( 'NONE',  ( 5.110351332421769754, 2.708615832122969191, 1.136051716722023208 ) ) ;
#6796 = CARTESIAN_POINT ( 'NONE',  ( -15.00000000000000000, 19.99999999999999645, 9.000000000000000000 ) ) ;
#6797 = CARTESIAN_POINT ( 'NONE',  ( 10.00000000000000000, 5.793104693147763662, 2.343061888689530026 ) ) ;
#6798 = EDGE_LOOP ( 'NONE', ( #8515, #5287, #6488, #4176, #10136, #105, #9634, #4010, #3746, #10150, #207, #7568 ) ) ;
#6799 = CARTESIAN_POINT ( 'NONE',  ( 4.444597532678119300, 0.7039550926810472786, 8.679999999999997939 ) ) ;
#6800 = CARTESIAN_POINT ( 'NONE',  ( -5.999999999999999112, -27.00000000000000711, -14.00000000000000178 ) ) ;
#6801 = EDGE_CURVE ( 'NONE', #5053, #10382, #3993, .T. ) ;
#6802 = EDGE_CURVE ( 'NONE', #8270, #2670, #1501, .T. ) ;
#6803 = CARTESIAN_POINT ( 'NONE',  ( -4.009529358847660596, 2.042957248827953265, 4.759999999999999787 ) ) ;
#6804 = CARTESIAN_POINT ( 'NONE',  ( -1.229367062500000163, -12.29022459553277002, -0.6354166673494632267 ) ) ;
#6805 = ORIENTED_EDGE ( 'NONE', *, *, #6651, .T. ) ;
#6806 = CARTESIAN_POINT ( 'NONE',  ( 0.000000000000000000, 0.000000000000000000, 0.000000000000000000 ) ) ;
#6807 = ORIENTED_EDGE ( 'NONE', *, *, #6371, .T. ) ;
#6808 = DIRECTION ( 'NONE',  ( 1.000000000000000000, -0.000000000000000000, -0.000000000000000000 ) ) ;
#6809 = DIRECTION ( 'NONE',  ( 0.000000000000000000, 0.000000000000000000, -1.000000000000000000 ) ) ;
#6810 = ORIENTED_EDGE ( 'NONE', *, *, #9762, .T. ) ;
#6811 = CARTESIAN_POINT ( 'NONE',  ( -3.889087296526005044, -3.889087296526019255, 12.59999999999999787 ) ) ;
#6812 = CARTESIAN_POINT ( 'NONE',  ( 3.889087296526005488, 3.889087296526018811, 11.19999999999999751 ) ) ;
#6813 = CARTESIAN_POINT ( 'NONE',  ( 0.8603895577212593571, 5.432285873273261068, 13.71999999999999886 ) ) ;
#6814 = ORIENTED_EDGE ( 'NONE', *, *, #3826, .F. ) ;
#6815 = EDGE_CURVE ( 'NONE', #9654, #9197, #8027, .T. ) ;
#6816 = CARTESIAN_POINT ( 'NONE',  ( -1.229367062500000385, -13.70977540446723886, -1.927083334016129745 ) ) ;
#6817 = VECTOR ( 'NONE', #249, 1000.000000000000000 ) ;
#6818 = SURFACE_STYLE_FILL_AREA ( #2062 ) ;
#6819 = VERTEX_POINT ( 'NONE', #5721 ) ;
#6820 = CARTESIAN_POINT ( 'NONE',  ( 16.97133164676619899, -10.00000000000000178, -12.00000000000000000 ) ) ;
#6821 = DIRECTION ( 'NONE',  ( -1.000000000000000000, -0.000000000000000000, -0.000000000000000000 ) ) ;
#6822 = VERTEX_POINT ( 'NONE', #5675 ) ;
#6823 = LINE ( 'NONE', #8380, #4548 ) ;
#6824 = CYLINDRICAL_SURFACE ( 'NONE', #4929, 3.000000000000000000 ) ;
#6825 = CYLINDRICAL_SURFACE ( 'NONE', #8787, 2.500000000000000000 ) ;
#6826 = CARTESIAN_POINT ( 'NONE',  ( 4.860232935257354114, -2.576046737280751842, -0.4360517167220233636 ) ) ;
#6828 = VERTEX_POINT ( 'NONE', #72 ) ;
#6827 = CIRCLE ( 'NONE', #6833, 6.248999999999999666 ) ;
#6829 = EDGE_CURVE ( 'NONE', #2259, #6218, #8608, .T. ) ;
#6830 = CARTESIAN_POINT ( 'NONE',  ( 0.4444353696672553311, -7.750000000000000000, -12.00000000000000000 ) ) ;
#6831 = CARTESIAN_POINT ( 'NONE',  ( -4.089228379062038066, 4.089228379062021190, 10.50000000000000000 ) ) ;
#6832 = LINE ( 'NONE', #5928, #8373 ) ;
#6833 = AXIS2_PLACEMENT_3D ( 'NONE', #9605, #7041, #6353 ) ;
#6834 = CARTESIAN_POINT ( 'NONE',  ( -0.7500000000000007772, -14.29903810567666156, -0.1666666666666669627 ) ) ;
#6835 = CARTESIAN_POINT ( 'NONE',  ( 8.980342580332745683, 3.750000000000000000, -12.00000000000000000 ) ) ;
#6836 = CARTESIAN_POINT ( 'NONE',  ( 0.1499999999999973577, 0.000000000000000000, 2.600000000000000089 ) ) ;
#6837 = CARTESIAN_POINT ( 'NONE',  ( 27.00000000000001066, -31.99999999999998579, -5.999999999999999112 ) ) ;
#6838 = CARTESIAN_POINT ( 'NONE',  ( 0.8323763977770604061, -4.658724279160015413, 10.37605171672202253 ) ) ;
#6839 =( BOUNDED_CURVE ( )  B_SPLINE_CURVE ( 2, ( #1750, #5866, #9071, #113, #7572, #1107, #1805 ),
 .UNSPECIFIED., .F., .F. ) 
 B_SPLINE_CURVE_WITH_KNOTS ( ( 3, 2, 2, 3 ),
 ( 0.5000000000000000000, 0.5277777777777777901, 0.5555555555555554692, 0.5833333333333332593 ),
 .UNSPECIFIED. ) 
 CURVE ( )  GEOMETRIC_REPRESENTATION_ITEM ( )  RATIONAL_B_SPLINE_CURVE ( ( 1.000000000000000000, 0.8660254037844387076, 1.000000000000000000, 0.8660254037844387076, 1.000000000000000000, 0.8660254037844392627, 0.9999999999999994449 ) ) 
 REPRESENTATION_ITEM ( '' )  );
#6840 = FACE_OUTER_BOUND ( 'NONE', #2627, .T. ) ;
#6841 = CARTESIAN_POINT ( 'NONE',  ( 0.6479879772514793856, -4.687928535947285091, 11.18394828327797441 ) ) ;
#6842 = CARTESIAN_POINT ( 'NONE',  ( -1.229367062500000163, -13.70977540446723708, -0.9270833340161298564 ) ) ;
#6843 = VECTOR ( 'NONE', #9172, 1000.000000000000000 ) ;
#6844 = ORIENTED_EDGE ( 'NONE', *, *, #3766, .T. ) ;
#6845 = DIRECTION ( 'NONE',  ( 0.000000000000000000, 0.000000000000000000, 1.000000000000000000 ) ) ;
#6846 = PRODUCT_DEFINITION_FORMATION_WITH_SPECIFIED_SOURCE ( 'ANY', '', #8677, .NOT_KNOWN. ) ;
#6847 = PLANE ( 'NONE',  #1968 ) ;
#6848 = EDGE_CURVE ( 'NONE', #2931, #2005, #3935, .T. ) ;
#6849 = CARTESIAN_POINT ( 'NONE',  ( 0.000000000000000000, -10.00000000000000000, -12.00000000000000000 ) ) ;
#6850 = ORIENTED_EDGE ( 'NONE', *, *, #10362, .F. ) ;
#6851 = VECTOR ( 'NONE', #892, 1000.000000000000000 ) ;
#6852 = CARTESIAN_POINT ( 'NONE',  ( -2.148092372876330813, -4.215868657802594122, 12.45999999999999730 ) ) ;
#6853 = CARTESIAN_POINT ( 'NONE',  ( 0.000000000000000000, 0.000000000000000000, -12.00000000000000000 ) ) ;
#6854 = CARTESIAN_POINT ( 'NONE',  ( -2.042957248827969252, 4.009529358847651714, 5.039999999999999147 ) ) ;
#6855 = CARTESIAN_POINT ( 'NONE',  ( 8.692241771943169307E-17, -11.58044919106553294, -1.218750000682796930 ) ) ;
#6856 = ORIENTED_EDGE ( 'NONE', *, *, #9750, .T. ) ;
#6857 = CARTESIAN_POINT ( 'NONE',  ( 0.000000000000000000, 0.000000000000000000, 0.000000000000000000 ) ) ;
#6858 = CIRCLE ( 'NONE', #3651, 2.500000000000000000 ) ;
#6859 = ORIENTED_EDGE ( 'NONE', *, *, #8247, .F. ) ;
#6860 = LINE ( 'NONE', #9308, #2135 ) ;
#6861 = AXIS2_PLACEMENT_3D ( 'NONE', #5095, #4451, #4295 ) ;
#6862 = DIRECTION ( 'NONE',  ( 0.000000000000000000, 0.000000000000000000, 1.000000000000000000 ) ) ;
#6863 = EDGE_CURVE ( 'NONE', #1777, #2162, #1632, .T. ) ;
#6864 = DIRECTION ( 'NONE',  ( 0.000000000000000000, -1.224646799147353207E-16, 1.000000000000000000 ) ) ;
#6865 = VERTEX_POINT ( 'NONE', #4835 ) ;
#6866 = CARTESIAN_POINT ( 'NONE',  ( -4.089228379062038066, 4.089228379062021190, 10.50000000000000000 ) ) ;
#6867 = CARTESIAN_POINT ( 'NONE',  ( 5.152728359536493663, 2.625446233515533745, 11.33999999999999808 ) ) ;
#6868 = CARTESIAN_POINT ( 'NONE',  ( 4.900535883036028828, -2.496947748567499126, 6.159999999999999254 ) ) ;
#6869 = VERTEX_POINT ( 'NONE', #915 ) ;
#6870 = PLANE ( 'NONE',  #4580 ) ;
#6871 = ORIENTED_EDGE ( 'NONE', *, *, #1169, .F. ) ;
#6872 = ADVANCED_FACE ( 'NONE', ( #8759 ), #10478, .T. ) ;
#6873 = DIRECTION ( 'NONE',  ( -1.000000000000000000, 0.000000000000000000, 0.000000000000000000 ) ) ;
#6874 = ADVANCED_FACE ( 'NONE', ( #5570 ), #9569, .T. ) ;
#6875 = DIRECTION ( 'NONE',  ( -0.7043149233066460235, 0.7043149233066439141, -0.08877487040322810941 ) ) ;
#6876 = ORIENTED_EDGE ( 'NONE', *, *, #4060, .F. ) ;
#6877 = ADVANCED_FACE ( 'NONE', ( #7163, #3194 ), #10420, .T. ) ;
#6878 = CYLINDRICAL_SURFACE ( 'NONE', #8965, 1.249999999999993339 ) ;
#6879 = DIRECTION ( 'NONE',  ( 1.000000000000000000, 0.000000000000000000, 0.000000000000000000 ) ) ;
#6880 = LINE ( 'NONE', #9275, #7940 ) ;
#6881 = CARTESIAN_POINT ( 'NONE',  ( 3.279728542977952799, -3.411736077305369541, 5.303948283277975406 ) ) ;
#6882 = ORIENTED_EDGE ( 'NONE', *, *, #2279, .F. ) ;
#6883 = CARTESIAN_POINT ( 'NONE',  ( -2.000000000000000000, 0.6700234925293845345, -8.473551116235670477 ) ) ;
#6884 = APPLICATION_CONTEXT ( 'automotive_design' ) ;
#6885 = CARTESIAN_POINT ( 'NONE',  ( -4.089228379062038066, 4.089228379062021190, 13.29999999999999538 ) ) ;
#6886 = CARTESIAN_POINT ( 'NONE',  ( -3.181725716174720991E-16, -14.73205080756888563, 0.3124999986344064173 ) ) ;
#6887 = EDGE_CURVE ( 'NONE', #2001, #7403, #9623, .T. ) ;
#6888 = LINE ( 'NONE', #6086, #766 ) ;
#6889 = DIRECTION ( 'NONE',  ( -1.000000000000000000, 0.000000000000000000, 0.000000000000000000 ) ) ;
#6890 = LINE ( 'NONE', #10044, #4161 ) ;
#6891 = LINE ( 'NONE', #4608, #2693 ) ;
#6892 = CARTESIAN_POINT ( 'NONE',  ( -3.411736077305382420, 3.279728542977939476, 11.49605171672201998 ) ) ;
#6893 = CARTESIAN_POINT ( 'NONE',  ( -0.6146835312500006365, -14.06466310670085562, -0.3854166673494634487 ) ) ;
#6894 = CARTESIAN_POINT ( 'NONE',  ( 0.8124729078102063129, -5.726445515403652209, 2.783948283277976277 ) ) ;
#6895 = CARTESIAN_POINT ( 'NONE',  ( -26.99999999999998934, -13.00000000000000533, -1.249999999999993339 ) ) ;
#6896 = ORIENTED_EDGE ( 'NONE', *, *, #7475, .T. ) ;
#6897 = CARTESIAN_POINT ( 'NONE',  ( -2.000000000000026645, 35.00000000000000000, -5.999999999999988454 ) ) ;
#6898 = LINE ( 'NONE', #596, #1037 ) ;
#6899 = CARTESIAN_POINT ( 'NONE',  ( 10.00000000000000000, 0.000000000000000000, 0.000000000000000000 ) ) ;
#6900 = DIRECTION ( 'NONE',  ( 0.000000000000000000, 0.000000000000000000, 1.000000000000000000 ) ) ;
#6901 = PRODUCT_RELATED_PRODUCT_CATEGORY ( 'part', '', ( #10292 ) ) ;
#6902 = ORIENTED_EDGE ( 'NONE', *, *, #6236, .T. ) ;
#6903 = CARTESIAN_POINT ( 'NONE',  ( -3.345732310141667831, 3.345732310141653620, 13.29999999999999716 ) ) ;
#6904 =( NAMED_UNIT ( * ) PLANE_ANGLE_UNIT ( ) SI_UNIT ( $, .RADIAN. ) );
#6905 = CARTESIAN_POINT ( 'NONE',  ( -2.148092372876330813, -4.215868657802593233, 6.859999999999999432 ) ) ;
#6906 = CARTESIAN_POINT ( 'NONE',  ( 8.692241771943169307E-17, -11.58044919106553294, -0.7187500006827969301 ) ) ;
#6907 = EDGE_LOOP ( 'NONE', ( #1065, #160, #3423, #1726, #3852, #4209, #6643, #1839, #364, #4023, #9154, #6550, #6383, #1961, #1552, #4753, #8783, #4639, #109, #6639, #9971, #621, #9911, #7374, #1026, #2299, #2100, #3053, #9357, #8862, #10032, #1269, #2573, #5770, #453, #5384 ) ) ;
#6908 = ORIENTED_EDGE ( 'NONE', *, *, #215, .F. ) ;
#6909 = CARTESIAN_POINT ( 'NONE',  ( 25.00000000000000000, -4.000000000000000000, -10.00000000000000000 ) ) ;
#6910 = CARTESIAN_POINT ( 'NONE',  ( 4.000000000000000888, 7.003298780661491918, -4.817032923780498521 ) ) ;
#6911 = LINE ( 'NONE', #2742, #181 ) ;
#6912 = ORIENTED_EDGE ( 'NONE', *, *, #4060, .T. ) ;
#6913 = CARTESIAN_POINT ( 'NONE',  ( -5.110351332421769754, -2.708615832122969191, 8.136051716722024096 ) ) ;
#6914 = CARTESIAN_POINT ( 'NONE',  ( -4.900535883036028828, 2.496947748567499126, 10.35999999999999943 ) ) ;
#6915 = VERTEX_POINT ( 'NONE', #8870 ) ;
#6916 = FACE_OUTER_BOUND ( 'NONE', #1751, .T. ) ;
#6917 = UNCERTAINTY_MEASURE_WITH_UNIT (LENGTH_MEASURE( 1.000000000000000082E-05 ), #251, 'distance_accuracy_value', 'NONE');
#6918 = ADVANCED_FACE ( 'NONE', ( #4041 ), #6575, .T. ) ;
#6919 = VERTEX_POINT ( 'NONE', #9885 ) ;
#6920 = ORIENTED_EDGE ( 'NONE', *, *, #4812, .F. ) ;
#6921 = FACE_BOUND ( 'NONE', #10417, .T. ) ;
#6922 = VECTOR ( 'NONE', #7738, 1000.000000000000000 ) ;
#6923 = DIRECTION ( 'NONE',  ( 0.7071067811865467956, 0.7071067811865484609, 0.000000000000000000 ) ) ;
#6924 = VERTEX_POINT ( 'NONE', #1818 ) ;
#6925 = CARTESIAN_POINT ( 'NONE',  ( 13.01080596966725622, -7.750000000000000000, -12.00000000000000000 ) ) ;
#6926 = LINE ( 'NONE', #2914, #9367 ) ;
#6927 = CARTESIAN_POINT ( 'NONE',  ( -3.244753828200538148, -3.119207202478392116, 6.003948283277975584 ) ) ;
#6928 = ORIENTED_EDGE ( 'NONE', *, *, #4469, .F. ) ;
#6929 = AXIS2_PLACEMENT_3D ( 'NONE', #8378, #10031, #3338 ) ;
#6930 = DIRECTION ( 'NONE',  ( 1.000000000000000000, 0.000000000000000000, 0.000000000000000000 ) ) ;
#6931 = ADVANCED_FACE ( 'NONE', ( #4993 ), #3408, .T. ) ;
#6932 = VECTOR ( 'NONE', #3160, 1000.000000000000000 ) ;
#6933 = EDGE_CURVE ( 'NONE', #505, #1349, #6858, .T. ) ;
#6934 = FACE_OUTER_BOUND ( 'NONE', #3090, .T. ) ;
#6935 = CARTESIAN_POINT ( 'NONE',  ( 0.7500000000000003331, -11.70096189432334732, 0.02083333196773980503 ) ) ;
#6936 = CARTESIAN_POINT ( 'NONE',  ( 3.000000000000000000, 1.959434878635765477E-16, 1.600000000000000311 ) ) ;
#6937 = CIRCLE ( 'NONE', #4396, 3.000000000000000000 ) ;
#6938 = CARTESIAN_POINT ( 'NONE',  ( -2.000000000000000000, -2.417132211460011337, -8.149077976821821778 ) ) ;
#6939 = DIRECTION ( 'NONE',  ( 1.000000000000000000, -0.000000000000000000, -0.000000000000000000 ) ) ;
#6940 = VECTOR ( 'NONE', #9734, 1000.000000000000000 ) ;
#6941 = DIRECTION ( 'NONE',  ( 1.000000000000000000, 0.000000000000000000, 0.000000000000000000 ) ) ;
#6942 = VECTOR ( 'NONE', #4652, 1000.000000000000000 ) ;
#6943 = DIRECTION ( 'NONE',  ( -1.000000000000000000, -0.000000000000000000, -0.000000000000000000 ) ) ;
#6944 = CARTESIAN_POINT ( 'NONE',  ( -2.122056237541221968, 3.969226411068977889, 14.43605171672202125 ) ) ;
#6945 = CARTESIAN_POINT ( 'NONE',  ( -1.229367062500000163, -12.29022459553277002, -1.635416667349463227 ) ) ;
#6946 = VECTOR ( 'NONE', #2035, 1000.000000000000000 ) ;
#6947 = EDGE_CURVE ( 'NONE', #7351, #4169, #6679, .T. ) ;
#6948 = AXIS2_PLACEMENT_3D ( 'NONE', #4887, #8187, #5724 ) ;
#6949 = CARTESIAN_POINT ( 'NONE',  ( -5.195105386651219348, -2.542276634908102295, 3.343948283277975886 ) ) ;
#6950 = CARTESIAN_POINT ( 'NONE',  ( 0.6146835312500001924, -11.93533689329915326, -1.135416667349463227 ) ) ;
#6952 = ORIENTED_EDGE ( 'NONE', *, *, #9804, .F. ) ;
#6951 = AXIS2_PLACEMENT_3D ( 'NONE', #3722, #5267, #4461 ) ;
#6953 = LINE ( 'NONE', #444, #2215 ) ;
#6954 = ADVANCED_FACE ( 'NONE', ( #329 ), #1124, .F. ) ;
#6955 = CARTESIAN_POINT ( 'NONE',  ( 10.69739119071655686, 6.025400000000000311, -12.00000000000000000 ) ) ;
#6956 = CARTESIAN_POINT ( 'NONE',  ( 30.00000000000001066, 0.000000000000000000, 0.000000000000000000 ) ) ;
#6957 = CARTESIAN_POINT ( 'NONE',  ( -2.000000000000000000, -1.471047635026825784, -6.892461014225975013 ) ) ;
#6958 = ORIENTED_EDGE ( 'NONE', *, *, #5191, .F. ) ;
#6959 = CARTESIAN_POINT ( 'NONE',  ( -9.000000000000000000, 19.99999999999999645, 15.00000000000000000 ) ) ;
#6960 = LINE ( 'NONE', #7921, #5086 ) ;
#6961 = CARTESIAN_POINT ( 'NONE',  ( 0.6162731882459174804, 4.458484982038668498, 14.71605171672202239 ) ) ;
#6962 = CARTESIAN_POINT ( 'NONE',  ( 0.6146835312499993043, -14.06466310670085562, -0.9270833340161300784 ) ) ;
#6963 = ORIENTED_EDGE ( 'NONE', *, *, #2986, .T. ) ;
#6964 = ORIENTED_EDGE ( 'NONE', *, *, #2847, .F. ) ;
#6965 = DIRECTION ( 'NONE',  ( 5.204170427930421283E-15, 0.000000000000000000, 1.000000000000000000 ) ) ;
#6966 = CARTESIAN_POINT ( 'NONE',  ( 30.00000000000001066, 35.00000000000001421, 9.000000000000000000 ) ) ;
#6967 = ORIENTED_EDGE ( 'NONE', *, *, #5527, .T. ) ;
#6968 = CARTESIAN_POINT ( 'NONE',  ( 5.110351332421769754, 2.708615832122969191, 6.736051716722023741 ) ) ;
#6969 = EDGE_CURVE ( 'NONE', #9821, #3947, #6632, .T. ) ;
#6970 = LINE ( 'NONE', #2209, #4733 ) ;
#6971 = ORIENTED_EDGE ( 'NONE', *, *, #6732, .T. ) ;
#6972 = FACE_BOUND ( 'NONE', #4366, .T. ) ;
#6973 = ORIENTED_EDGE ( 'NONE', *, *, #7796, .F. ) ;
#6974 = ADVANCED_FACE ( 'NONE', ( #8288 ), #7490, .T. ) ;
#6975 = FILL_AREA_STYLE ('',( #5230 ) ) ;
#6976 = ORIENTED_EDGE ( 'NONE', *, *, #1498, .T. ) ;
#6977 = FACE_BOUND ( 'NONE', #3358, .T. ) ;
#6978 = CARTESIAN_POINT ( 'NONE',  ( -1.500000000000000222, -13.00000000000000533, -0.2500000000000002220 ) ) ;
#6979 = ORIENTED_EDGE ( 'NONE', *, *, #81, .T. ) ;
#6980 = CARTESIAN_POINT ( 'NONE',  ( 10.00000000000000000, 0.000000000000000000, 0.000000000000000000 ) ) ;
#6981 = EDGE_CURVE ( 'NONE', #8011, #7252, #8393, .T. ) ;
#6982 = DIRECTION ( 'NONE',  ( -1.000000000000000000, 0.000000000000000000, -0.000000000000000000 ) ) ;
#6983 = CARTESIAN_POINT ( 'NONE',  ( 4.860232935257354114, -2.576046737280751842, 7.963948283277976437 ) ) ;
#6984 = ORIENTED_EDGE ( 'NONE', *, *, #8249, .T. ) ;
#6985 = CARTESIAN_POINT ( 'NONE',  ( -1.500000000000000222, -13.00000000000000533, -0.3125000013655936937 ) ) ;
#6986 = AXIS2_PLACEMENT_3D ( 'NONE', #7144, #5449, #8638 ) ;
#6987 = DIRECTION ( 'NONE',  ( 0.000000000000000000, 1.000000000000000000, 0.000000000000000000 ) ) ;
#6988 = DIRECTION ( 'NONE',  ( 0.000000000000000000, 0.000000000000000000, 1.000000000000000000 ) ) ;
#6989 = PLANE ( 'NONE',  #1354 ) ;
#6990 = AXIS2_PLACEMENT_3D ( 'NONE', #8144, #7439, #2622 ) ;
#6991 = CARTESIAN_POINT ( 'NONE',  ( 10.00000000000000000, -6.700937042937042065, -2.183447440113260196 ) ) ;
#6992 = PLANE ( 'NONE',  #8912 ) ;
#6993 = ADVANCED_FACE ( 'NONE', ( #283 ), #231, .T. ) ;
#6994 = DIRECTION ( 'NONE',  ( -0.3420201433256627732, -0.9396926207859105373, 0.000000000000000000 ) ) ;
#6995 = CARTESIAN_POINT ( 'NONE',  ( 2.042957248827968808, -4.009529358847652603, 9.240000000000000213 ) ) ;
#6996 = CARTESIAN_POINT ( 'NONE',  ( 0.6146835312499993043, -14.06466310670085562, -0.3020833340161297453 ) ) ;
#6997 = CARTESIAN_POINT ( 'NONE',  ( -5.697241258616385196, 0.9968613283357647958, 12.02394828327797427 ) ) ;
#6998 = CIRCLE ( 'NONE', #9899, 2.399999999999999911 ) ;
#6999 = CARTESIAN_POINT ( 'NONE',  ( 0.6146835312500001924, -11.93533689329915326, -1.635416667349463227 ) ) ;
#7000 = EDGE_LOOP ( 'NONE', ( #5593, #8062, #2140, #9378 ) ) ;
#7001 = CARTESIAN_POINT ( 'NONE',  ( -2.000000000000000000, 0.005878491403557128264, -7.047692205288322853 ) ) ;
#7002 = EDGE_CURVE ( 'NONE', #6339, #7874, #1015, .T. ) ;
#7003 = DIRECTION ( 'NONE',  ( 0.000000000000000000, -1.000000000000000000, 0.000000000000000000 ) ) ;
#7004 = DIRECTION ( 'NONE',  ( 0.000000000000000000, 0.000000000000000000, 1.000000000000000000 ) ) ;
#7005 = EDGE_CURVE ( 'NONE', #5519, #8221, #7429, .T. ) ;
#7006 = DIRECTION ( 'NONE',  ( -0.000000000000000000, -0.000000000000000000, 1.000000000000000000 ) ) ;
#7007 = EDGE_LOOP ( 'NONE', ( #2158, #6807, #192, #1084, #2946, #9209, #9645, #1844, #5171, #4364, #4961, #3014 ) ) ;
#7008 = SURFACE_SIDE_STYLE ('',( #7116 ) ) ;
#7009 = VECTOR ( 'NONE', #7315, 1000.000000000000000 ) ;
#7010 = CARTESIAN_POINT ( 'NONE',  ( 4.009529358847659708, -2.042957248827953709, 11.75999999999999979 ) ) ;
#7011 = CARTESIAN_POINT ( 'NONE',  ( -0.6146835312499998594, -11.93533689329915326, -0.6770833340161300784 ) ) ;
#7012 = EDGE_LOOP ( 'NONE', ( #3629, #9462, #4188, #1536 ) ) ;
#7013 = EDGE_LOOP ( 'NONE', ( #827, #8045, #6008, #9859 ) ) ;
#7014 = EDGE_CURVE ( 'NONE', #8945, #10382, #8343, .T. ) ;
#7015 = CARTESIAN_POINT ( 'NONE',  ( -2.000000000000026645, 35.00000000000000000, 5.999999999999987566 ) ) ;
#7016 = AXIS2_PLACEMENT_3D ( 'NONE', #5248, #582, #380 ) ;
#7017 = CARTESIAN_POINT ( 'NONE',  ( -2.000000000000000000, 6.100541242131515496, -3.528937025535514138 ) ) ;
#7018 = ORIENTED_EDGE ( 'NONE', *, *, #4683, .T. ) ;
#7019 = CARTESIAN_POINT ( 'NONE',  ( 4.155232146225751322, -4.023224611898307934, 7.296051716722023350 ) ) ;
#7020 = AXIS2_PLACEMENT_3D ( 'NONE', #1194, #1142, #4365 ) ;
#7021 = DIRECTION ( 'NONE',  ( 1.000000000000000000, -0.000000000000000000, -0.000000000000000000 ) ) ;
#7022 = VERTEX_POINT ( 'NONE', #1976 ) ;
#7023 = FACE_OUTER_BOUND ( 'NONE', #9056, .T. ) ;
#7024 = AXIS2_PLACEMENT_3D ( 'NONE', #1636, #9595, #7889 ) ;
#7025 = VERTEX_POINT ( 'NONE', #2563 ) ;
#7026 =( LENGTH_UNIT ( ) NAMED_UNIT ( * ) SI_UNIT ( .MILLI., .METRE. ) );
#7027 = AXIS2_PLACEMENT_3D ( 'NONE', #1336, #3570, #10154 ) ;
#7028 = ORIENTED_EDGE ( 'NONE', *, *, #9938, .F. ) ;
#7029 = CARTESIAN_POINT ( 'NONE',  ( 1.300000000000000044, 0.000000000000000000, 0.000000000000000000 ) ) ;
#7030 = CARTESIAN_POINT ( 'NONE',  ( -5.999999999999999112, -27.00000000000000711, -17.00000000000000000 ) ) ;
#7031 = ORIENTED_EDGE ( 'NONE', *, *, #9490, .T. ) ;
#7032 = DIRECTION ( 'NONE',  ( 1.000000000000000000, -0.000000000000000000, -0.000000000000000000 ) ) ;
#7033 = AXIS2_PLACEMENT_3D ( 'NONE', #3142, #811, #6369 ) ;
#7034 = CARTESIAN_POINT ( 'NONE',  ( 16.98057649071655817, -10.02539999999999942, -12.00000000000000000 ) ) ;
#7035 = ADVANCED_FACE ( 'NONE', ( #3506 ), #2614, .T. ) ;
#7036 = CARTESIAN_POINT ( 'NONE',  ( 0.9480714621563713917, 5.418398423912717199, 4.323948283277975868 ) ) ;
#7037 = ORIENTED_EDGE ( 'NONE', *, *, #8514, .T. ) ;
#7038 = VECTOR ( 'NONE', #1170, 1000.000000000000000 ) ;
#7039 = CARTESIAN_POINT ( 'NONE',  ( -2.000000000000000000, -6.700937042937042065, 0.8165525598867396928 ) ) ;
#7040 = LINE ( 'NONE', #3807, #3120 ) ;
#7041 = DIRECTION ( 'NONE',  ( -1.000000000000000000, -0.000000000000000000, -0.000000000000000000 ) ) ;
#7042 = CARTESIAN_POINT ( 'NONE',  ( -2.000000000000000000, -6.200809695932771426, -0.7745709230445765314 ) ) ;
#7043 = DIRECTION ( 'NONE',  ( 0.000000000000000000, 0.000000000000000000, 1.000000000000000000 ) ) ;
#7044 = FACE_BOUND ( 'NONE', #6183, .T. ) ;
#7045 = DIRECTION ( 'NONE',  ( 0.000000000000000000, 0.000000000000000000, -1.000000000000000000 ) ) ;
#7046 = DIRECTION ( 'NONE',  ( 0.000000000000000000, 0.000000000000000000, -1.000000000000000000 ) ) ;
#7047 = CARTESIAN_POINT ( 'NONE',  ( -4.009529358847660596, 2.042957248827953265, 10.35999999999999943 ) ) ;
#7048 = CARTESIAN_POINT ( 'NONE',  ( 1.229367062500000163, -13.00000000000000533, 0.2812499993172035695 ) ) ;
#7049 = CARTESIAN_POINT ( 'NONE',  ( 4.023224611898322145, -4.155232146225737111, 5.303948283277975406 ) ) ;
#7050 = DIRECTION ( 'NONE',  ( 0.000000000000000000, -0.000000000000000000, 1.000000000000000000 ) ) ;
#7051 = ADVANCED_FACE ( 'NONE', ( #6724 ), #9986, .T. ) ;
#7052 = ORIENTED_EDGE ( 'NONE', *, *, #6053, .F. ) ;
#7053 = APPLICATION_PROTOCOL_DEFINITION ( 'draft international standard', 'automotive_design', 1998, #9953 ) ;
#7054 = DIRECTION ( 'NONE',  ( 1.000000000000000000, -0.000000000000000000, -0.000000000000000000 ) ) ;
#7055 = LINE ( 'NONE', #7861, #7467 ) ;
#7056 = CARTESIAN_POINT ( 'NONE',  ( 0.000000000000000000, -13.00000000000000533, -3.000000000000000000 ) ) ;
#7057 = DIRECTION ( 'NONE',  ( 0.000000000000000000, 0.000000000000000000, -1.000000000000000000 ) ) ;
#7058 = PRODUCT_DEFINITION_SHAPE ( 'NONE', 'NONE',  #1276 ) ;
#7059 = ORIENTED_EDGE ( 'NONE', *, *, #3507, .T. ) ;
#7060 = LINE ( 'NONE', #10310, #8123 ) ;
#7061 = CYLINDRICAL_SURFACE ( 'NONE', #9147, 2.000000000000000000 ) ;
#7062 = CARTESIAN_POINT ( 'NONE',  ( 4.009529358847659708, -2.042957248827953709, 8.959999999999999076 ) ) ;
#7063 = ADVANCED_FACE ( 'NONE', ( #5196, #8441 ), #4398, .T. ) ;
#7064 = CARTESIAN_POINT ( 'NONE',  ( -1.500000000000000000, -12.13397459621556607, -0.2916666666666666852 ) ) ;
#7065 = EDGE_CURVE ( 'NONE', #7761, #2162, #483, .T. ) ;
#7066 = ORIENTED_EDGE ( 'NONE', *, *, #2232, .T. ) ;
#7067 = VERTEX_POINT ( 'NONE', #9393 ) ;
#7068 = CARTESIAN_POINT ( 'NONE',  ( -2.000000000000000000, 0.000000000000000000, 0.000000000000000000 ) ) ;
#7069 = CARTESIAN_POINT ( 'NONE',  ( 0.7500000000000003331, -11.70096189432334732, -2.479166668032260379 ) ) ;
#7070 = VERTEX_POINT ( 'NONE', #2235 ) ;
#7071 = CARTESIAN_POINT ( 'NONE',  ( -3.826313983664925811, -3.951860609387098489, 7.996051716722022640 ) ) ;
#7072 = DIRECTION ( 'NONE',  ( 0.000000000000000000, -0.000000000000000000, 1.000000000000000000 ) ) ;
#7073 = CARTESIAN_POINT ( 'NONE',  ( 0.000000000000000000, 3.750000000000000000, -12.00000000000000000 ) ) ;
#7074 = ORIENTED_EDGE ( 'NONE', *, *, #7634, .F. ) ;
#7075 = DIRECTION ( 'NONE',  ( 1.000000000000000000, -0.000000000000000000, 0.000000000000000000 ) ) ;
#7076 = CARTESIAN_POINT ( 'NONE',  ( 5.418398423912711870, 0.9480714621563913758, 9.676051716722021467 ) ) ;
#7077 = EDGE_CURVE ( 'NONE', #4407, #1730, #8644, .T. ) ;
#7078 = ORIENTED_EDGE ( 'NONE', *, *, #9315, .T. ) ;
#7079 = ORIENTED_EDGE ( 'NONE', *, *, #10108, .T. ) ;
#7080 = LINE ( 'NONE', #8844, #271 ) ;
#7081 = AXIS2_PLACEMENT_3D ( 'NONE', #10144, #2079, #5305 ) ;
#7082 = FACE_OUTER_BOUND ( 'NONE', #593, .T. ) ;
#7083 = ORIENTED_EDGE ( 'NONE', *, *, #3509, .T. ) ;
#7084 = CARTESIAN_POINT ( 'NONE',  ( 10.00000000000000000, 4.137773741518453008, -5.705158055754754542 ) ) ;
#7085 = DIRECTION ( 'NONE',  ( 0.000000000000000000, 0.000000000000000000, -1.000000000000000000 ) ) ;
#7086 = CARTESIAN_POINT ( 'NONE',  ( 0.8124729078102063129, -5.726445515403652209, 2.783948283277976277 ) ) ;
#7087 = ORIENTED_EDGE ( 'NONE', *, *, #9219, .T. ) ;
#7088 = CARTESIAN_POINT ( 'NONE',  ( -1.500000000000000000, -12.13397459621556607, -1.854166668032260157 ) ) ;
#7089 = CARTESIAN_POINT ( 'NONE',  ( 0.7500000000000003331, -11.70096189432334732, -0.4791666680322602123 ) ) ;
#7090 = CARTESIAN_POINT ( 'NONE',  ( 0.000000000000000000, 0.000000000000000000, 0.000000000000000000 ) ) ;
#7091 = VECTOR ( 'NONE', #4234, 1000.000000000000000 ) ;
#7092 = PRODUCT_RELATED_PRODUCT_CATEGORY ( 'part', '', ( #7331 ) ) ;
#7093 = CARTESIAN_POINT ( 'NONE',  ( 8.980342580332745683, -7.750000000000000000, -12.00000000000000000 ) ) ;
#7094 = CIRCLE ( 'NONE', #5901, 4.000000000000000000 ) ;
#7095 = CARTESIAN_POINT ( 'NONE',  ( 0.000000000000000000, -1.478016689125442706, 1.843143693225357538E-15 ) ) ;
#7096 = DIRECTION ( 'NONE',  ( 0.000000000000000000, 0.000000000000000000, 1.000000000000000000 ) ) ;
#7097 = CARTESIAN_POINT ( 'NONE',  ( 1.499999999999999778, -13.86602540378444637, -1.041666666666666963 ) ) ;
#7098 = AXIS2_PLACEMENT_3D ( 'NONE', #8480, #1365, #1264 ) ;
#7099 = CARTESIAN_POINT ( 'NONE',  ( 10.00000000000000000, 5.471841788314748989, -3.018103451449677621 ) ) ;
#7100 = CARTESIAN_POINT ( 'NONE',  ( -3.345732310141667831, 3.345732310141653620, 4.900000000000000355 ) ) ;
#7101 = COLOUR_RGB ( '', 0.72549020, 0.75294118, 0.79215686) ;
#7102 = CARTESIAN_POINT ( 'NONE',  ( 1.229367062499999719, -13.70977540446724063, -2.385416667349463005 ) ) ;
#7103 = CARTESIAN_POINT ( 'NONE',  ( 3.951860609387084722, 3.826313983664940022, 4.603948283277976117 ) ) ;
#7104 = LINE ( 'NONE', #641, #7842 ) ;
#7105 = AXIS2_PLACEMENT_3D ( 'NONE', #10220, #1252, #7724 ) ;
#7106 = ORIENTED_EDGE ( 'NONE', *, *, #4867, .F. ) ;
#7107 = EDGE_CURVE ( 'NONE', #5694, #5003, #584, .T. ) ;
#7108 = DIRECTION ( 'NONE',  ( 0.000000000000000000, 0.000000000000000000, 1.000000000000000000 ) ) ;
#7109 = CARTESIAN_POINT ( 'NONE',  ( -1.500000000000000666, -13.86602540378444637, -0.7083333333333333703 ) ) ;
#7110 = DIRECTION ( 'NONE',  ( -1.000000000000000000, -0.000000000000000000, -0.000000000000000000 ) ) ;
#7111 = DIRECTION ( 'NONE',  ( 0.000000000000000000, 0.000000000000000000, 1.000000000000000000 ) ) ;
#7112 = LINE ( 'NONE', #10370, #522 ) ;
#7113 = ORIENTED_EDGE ( 'NONE', *, *, #4140, .T. ) ;
#7114 = VECTOR ( 'NONE', #3672, 1000.000000000000000 ) ;
#7115 = EDGE_CURVE ( 'NONE', #3788, #8270, #10092, .T. ) ;
#7116 = SURFACE_STYLE_FILL_AREA ( #3884 ) ;
#7117 = CARTESIAN_POINT ( 'NONE',  ( 20.12216914071655793, -10.02539999999999942, -12.00000000000000000 ) ) ;
#7118 = CARTESIAN_POINT ( 'NONE',  ( 3.181980515339458471, 3.181980515339470461, 13.99999999999999822 ) ) ;
#7119 = CIRCLE ( 'NONE', #4746, 2.399999999999999911 ) ;
#7120 = CARTESIAN_POINT ( 'NONE',  ( 1.500000000000000000, -13.86602540378444459, -1.541666666666666963 ) ) ;
#7121 = ORIENTED_EDGE ( 'NONE', *, *, #859, .T. ) ;
#7122 = CIRCLE ( 'NONE', #691, 8.500000000000000000 ) ;
#7123 = ORIENTED_EDGE ( 'NONE', *, *, #1260, .F. ) ;
#7124 = DIRECTION ( 'NONE',  ( -1.000000000000000000, -0.000000000000000000, -0.000000000000000000 ) ) ;
#7125 = ORIENTED_EDGE ( 'NONE', *, *, #8184, .F. ) ;
#7126 = ADVANCED_FACE ( 'NONE', ( #2178 ), #8729, .T. ) ;
#7127 = CARTESIAN_POINT ( 'NONE',  ( 3.826313983664925811, 3.951860609387098044, 12.19605171672202282 ) ) ;
#7128 = ADVANCED_FACE ( 'NONE', ( #8494 ), #4606, .F. ) ;
#7129 = LINE ( 'NONE', #7880, #9295 ) ;
#7130 = CARTESIAN_POINT ( 'NONE',  ( 11.30300220323380600, 6.000000000000000000, -12.00000000000000000 ) ) ;
#7131 = ORIENTED_EDGE ( 'NONE', *, *, #8550, .F. ) ;
#7132 = LINE ( 'NONE', #3903, #10026 ) ;
#7133 = CARTESIAN_POINT ( 'NONE',  ( 4.049832306626335310, -1.963858260114701215, 1.556051716722023581 ) ) ;
#7134 = ORIENTED_EDGE ( 'NONE', *, *, #845, .F. ) ;
#7135 = LINE ( 'NONE', #3963, #2467 ) ;
#7136 = DIRECTION ( 'NONE',  ( 0.000000000000000000, 0.000000000000000000, 1.000000000000000000 ) ) ;
#7137 = ORIENTED_EDGE ( 'NONE', *, *, #2428, .F. ) ;
#7138 = EDGE_CURVE ( 'NONE', #247, #2213, #3661, .T. ) ;
#7139 = FACE_OUTER_BOUND ( 'NONE', #5993, .T. ) ;
#7140 = DIRECTION ( 'NONE',  ( -1.000000000000000000, -0.000000000000000000, -0.000000000000000000 ) ) ;
#7141 = CARTESIAN_POINT ( 'NONE',  ( -5.446173322633801384, -0.7727076532861678615, 6.283948283277974944 ) ) ;
#7142 = ORIENTED_EDGE ( 'NONE', *, *, #2937, .F. ) ;
#7143 = CARTESIAN_POINT ( 'NONE',  ( -0.6146835312500006365, -14.06466310670085562, -2.385416667349463005 ) ) ;
#7144 = CARTESIAN_POINT ( 'NONE',  ( -2.000000000000000000, -7.009698679648282749, -0.7308381473897593850 ) ) ;
#7145 = LINE ( 'NONE', #3757, #6661 ) ;
#7146 = ORIENTED_EDGE ( 'NONE', *, *, #7412, .F. ) ;
#7147 = PRODUCT_DEFINITION_SHAPE ( 'NONE', 'NONE',  #6123 ) ;
#7148 = CARTESIAN_POINT ( 'NONE',  ( 1.500000000000000222, -13.00000000000000533, -0.5625000013655934161 ) ) ;
#7149 = LINE ( 'NONE', #10408, #4399 ) ;
#7150 = LINE ( 'NONE', #3078, #8972 ) ;
#7151 = ADVANCED_FACE ( 'NONE', ( #3760 ), #8695, .F. ) ;
#7152 = DIRECTION ( 'NONE',  ( 0.000000000000000000, 0.000000000000000000, 1.000000000000000000 ) ) ;
#7153 = VECTOR ( 'NONE', #9498, 1000.000000000000000 ) ;
#7154 = LINE ( 'NONE', #1550, #1164 ) ;
#7155 = CARTESIAN_POINT ( 'NONE',  ( -2.042957248827969252, 4.009529358847651714, 7.839999999999999858 ) ) ;
#7156 = CARTESIAN_POINT ( 'NONE',  ( -1.229367062500000163, -13.00000000000000533, -0.5937500006827968191 ) ) ;
#7157 = CARTESIAN_POINT ( 'NONE',  ( 2.708615832122949652, 5.110351332421781301, 7.263948283277976259 ) ) ;
#7158 = FACE_BOUND ( 'NONE', #4419, .T. ) ;
#7159 = ORIENTED_EDGE ( 'NONE', *, *, #9703, .T. ) ;
#7160 = CIRCLE ( 'NONE', #5638, 8.500000000000000000 ) ;
#7161 = CONTEXT_DEPENDENT_SHAPE_REPRESENTATION ( #1676, #2510 ) ;
#7162 = CARTESIAN_POINT ( 'NONE',  ( -5.152728359536494551, -2.625446233515535521, 1.540000000000000036 ) ) ;
#7163 = FACE_BOUND ( 'NONE', #500, .T. ) ;
#7164 = VERTEX_POINT ( 'NONE', #1431 ) ;
#7165 = DIRECTION ( 'NONE',  ( 0.000000000000000000, 0.000000000000000000, -1.000000000000000000 ) ) ;
#7166 = PLANE ( 'NONE',  #3404 ) ;
#7167 = DIRECTION ( 'NONE',  ( 0.000000000000000000, 0.000000000000000000, 1.000000000000000000 ) ) ;
#7168 = DIRECTION ( 'NONE',  ( -0.000000000000000000, 1.000000000000000000, -0.000000000000000000 ) ) ;
#7169 = ADVANCED_FACE ( 'NONE', ( #1324 ), #6244, .F. ) ;
#7170 = DIRECTION ( 'NONE',  ( 0.3420201433256627732, -0.9396926207859105373, 0.000000000000000000 ) ) ;
#7171 = COLOUR_RGB ( '', 0.40784314, 0.44705882, 0.49803922) ;
#7172 = CARTESIAN_POINT ( 'NONE',  ( -0.7401821875142701179, 4.673326407553649808, 13.57999999999999474 ) ) ;
#7173 = PRODUCT_DEFINITION_CONTEXT ( 'detailed design', #10015, 'design' ) ;
#7174 = CARTESIAN_POINT ( 'NONE',  ( -3.181725716174720498E-16, -14.73205080756888385, -1.625000000000000222 ) ) ;
#7175 = ORIENTED_EDGE ( 'NONE', *, *, #10362, .T. ) ;
#7176 = ADVANCED_FACE ( 'NONE', ( #5303 ), #1225, .F. ) ;
#7177 = ORIENTED_EDGE ( 'NONE', *, *, #3704, .T. ) ;
#7178 = VECTOR ( 'NONE', #6987, 1000.000000000000000 ) ;
#7179 = LINE ( 'NONE', #10435, #9163 ) ;
#7180 = LINE ( 'NONE', #3787, #3225 ) ;
#7181 = VERTEX_POINT ( 'NONE', #3024 ) ;
#7182 = DIRECTION ( 'NONE',  ( 0.8660254037844402619, -0.000000000000000000, 0.4999999999999972244 ) ) ;
#7183 = DIRECTION ( 'NONE',  ( 0.000000000000000000, 0.000000000000000000, 1.000000000000000000 ) ) ;
#7184 = ORIENTED_EDGE ( 'NONE', *, *, #9661, .T. ) ;
#7185 =( BOUNDED_CURVE ( )  B_SPLINE_CURVE ( 2, ( #2179, #6197, #5457, #5402, #8804, #7097, #8646 ),
 .UNSPECIFIED., .F., .T. ) 
 B_SPLINE_CURVE_WITH_KNOTS ( ( 3, 2, 2, 3 ),
 ( 0.5833333333333332593, 0.6111111111111110494, 0.6388888888888888395, 0.6666666666666666297 ),
 .UNSPECIFIED. ) 
 CURVE ( )  GEOMETRIC_REPRESENTATION_ITEM ( )  RATIONAL_B_SPLINE_CURVE ( ( 1.000000000000000444, 0.8660254037844381525, 1.000000000000000000, 0.8660254037844387076, 1.000000000000000000, 0.8660254037844387076, 1.000000000000000000 ) ) 
 REPRESENTATION_ITEM ( '' )  );
#7186 = CARTESIAN_POINT ( 'NONE',  ( 25.00000000000000000, -4.000000000000000000, -12.00000000000000000 ) ) ;
#7187 = CARTESIAN_POINT ( 'NONE',  ( -4.049832306626335310, 1.963858260114700327, 2.956051716722023492 ) ) ;
#7188 = VERTEX_POINT ( 'NONE', #2976 ) ;
#7189 = AXIS2_PLACEMENT_3D ( 'NONE', #4655, #10463, #6242 ) ;
#7190 = EDGE_CURVE ( 'NONE', #10128, #307, #6143, .T. ) ;
#7191 = CYLINDRICAL_SURFACE ( 'NONE', #7545, 6.248999999999999666 ) ;
#7192 = PRODUCT_DEFINITION_FORMATION_WITH_SPECIFIED_SOURCE ( 'ANY', '', #4517, .NOT_KNOWN. ) ;
#7193 = EDGE_CURVE ( 'NONE', #2528, #8329, #1973, .T. ) ;
#7194 = DIRECTION ( 'NONE',  ( 1.000000000000000000, 0.000000000000000000, 0.000000000000000000 ) ) ;
#7195 = VERTEX_POINT ( 'NONE', #5250 ) ;
#7196 = CARTESIAN_POINT ( 'NONE',  ( 4.900535883036028828, -2.496947748567499126, 0.5599999999999999423 ) ) ;
#7197 = FACE_OUTER_BOUND ( 'NONE', #3700, .T. ) ;
#7198 = CARTESIAN_POINT ( 'NONE',  ( -0.9480714621563718358, -5.418398423912716311, 2.923948283277976401 ) ) ;
#7199 = ORIENTED_EDGE ( 'NONE', *, *, #7611, .F. ) ;
#7200 = VECTOR ( 'NONE', #5854, 1000.000000000000000 ) ;
#7201 = CARTESIAN_POINT ( 'NONE',  ( -1.500000000000000222, -13.00000000000000533, -0.3125000013655936937 ) ) ;
#7202 = CARTESIAN_POINT ( 'NONE',  ( 17.00000000000000000, 19.99999999999999645, -9.000000000000000000 ) ) ;
#7203 = ADVANCED_FACE ( 'NONE', ( #10244, #7044, #8593 ), #4553, .T. ) ;
#7204 = CARTESIAN_POINT ( 'NONE',  ( 1.229367062500000163, -13.00000000000000533, -2.781250000682796486 ) ) ;
#7205 = EDGE_CURVE ( 'NONE', #897, #9050, #111, .T. ) ;
#7206 = ORIENTED_EDGE ( 'NONE', *, *, #5117, .F. ) ;
#7207 = SHAPE_REPRESENTATION ( 'socket head cap screw_iso_ISO 4762 M3 x 8 - 8N', ( #2101 ), #1104 ) ;
#7208 = CARTESIAN_POINT ( 'NONE',  ( 3.099999999999998757, 0.000000000000000000, 0.000000000000000000 ) ) ;
#7209 = VECTOR ( 'NONE', #5351, 1000.000000000000000 ) ;
#7210 = LINE ( 'NONE', #4128, #3732 ) ;
#7211 = DIRECTION ( 'NONE',  ( -1.000000000000000000, -0.000000000000000000, -0.000000000000000000 ) ) ;
#7212 = CARTESIAN_POINT ( 'NONE',  ( 2.697157280332745266, 3.750000000000000000, -12.00000000000000000 ) ) ;
#7213 = VECTOR ( 'NONE', #7382, 1000.000000000000000 ) ;
#7214 = DIRECTION ( 'NONE',  ( 1.156482317317871478E-16, -1.000000000000000000, -0.000000000000000000 ) ) ;
#7215 = CARTESIAN_POINT ( 'NONE',  ( 4.215868657802586128, 2.148092372876346801, 5.739999999999997549 ) ) ;
#7216 = EDGE_LOOP ( 'NONE', ( #2107, #954, #4962, #6408 ) ) ;
#7217 = CARTESIAN_POINT ( 'NONE',  ( 23.26376179071655770, -10.02539999999999942, -12.00000000000000000 ) ) ;
#7218 = CARTESIAN_POINT ( 'NONE',  ( 0.8124729078102063129, -5.726445515403652209, 8.383948283277975477 ) ) ;
#7219 = ADVANCED_FACE ( 'NONE', ( #5456 ), #6531, .T. ) ;
#7220 = CARTESIAN_POINT ( 'NONE',  ( 0.000000000000000000, 6.000000000000000000, -12.00000000000000000 ) ) ;
#7221 = ORIENTED_EDGE ( 'NONE', *, *, #3850, .T. ) ;
#7222 = ITEM_DEFINED_TRANSFORMATION ( 'NONE', 'NONE', #9919,  #2101 ) ;
#7223 = LINE ( 'NONE', #4783, #2121 ) ;
#7224 = CARTESIAN_POINT ( 'NONE',  ( -2.000000000000000000, 7.008469740302810891, -0.7425307242147085596 ) ) ;
#7225 = ORIENTED_EDGE ( 'NONE', *, *, #9880, .T. ) ;
#7226 = DIRECTION ( 'NONE',  ( 1.000000000000000000, 0.000000000000000000, 0.000000000000000000 ) ) ;
#7227 = DIRECTION ( 'NONE',  ( 1.000000000000000000, 0.000000000000000000, 0.000000000000000000 ) ) ;
#7228 = DIRECTION ( 'NONE',  ( 1.000000000000000000, 0.000000000000000000, 0.000000000000000000 ) ) ;
#7229 = DIRECTION ( 'NONE',  ( 0.7071067811865467956, 0.7071067811865484609, -6.099057733344262077E-17 ) ) ;
#7230 = CARTESIAN_POINT ( 'NONE',  ( -10.00000000000000000, 0.000000000000000000, 0.000000000000000000 ) ) ;
#7231 = CARTESIAN_POINT ( 'NONE',  ( 0.6479879772514793856, -4.687928535947285091, -0.01605171672202330979 ) ) ;
#7232 = CARTESIAN_POINT ( 'NONE',  ( 1.500000000000000000, -13.86602540378444459, -0.5416666666666668517 ) ) ;
#7233 = ORIENTED_EDGE ( 'NONE', *, *, #2998, .T. ) ;
#7234 = ORIENTED_EDGE ( 'NONE', *, *, #2801, .F. ) ;
#7235 = PRODUCT_DEFINITION ( 'UNKNOWN', '', #9232, #4731 ) ;
#7236 = CARTESIAN_POINT ( 'NONE',  ( -29.99999999999998934, 0.000000000000000000, 1.599999999999998979 ) ) ;
#7237 = PLANE ( 'NONE',  #3894 ) ;
#7238 = ORIENTED_EDGE ( 'NONE', *, *, #3676, .T. ) ;
#7239 = CARTESIAN_POINT ( 'NONE',  ( 0.7039550926810297371, 4.444597532678122853, 2.519999999999999574 ) ) ;
#7240 = LINE ( 'NONE', #9795, #3386 ) ;
#7241 = ORIENTED_EDGE ( 'NONE', *, *, #4537, .F. ) ;
#7242 = CARTESIAN_POINT ( 'NONE',  ( -0.7727076532861475444, -5.446173322633804048, 13.31605171672202204 ) ) ;
#7243 = ORIENTED_EDGE ( 'NONE', *, *, #8229, .T. ) ;
#7244 = FILL_AREA_STYLE ('',( #7300 ) ) ;
#7245 = LINE ( 'NONE', #2321, #1955 ) ;
#7246 = FACE_OUTER_BOUND ( 'NONE', #1008, .T. ) ;
#7247 = ORIENTED_EDGE ( 'NONE', *, *, #9678, .T. ) ;
#7248 =( BOUNDED_CURVE ( )  B_SPLINE_CURVE ( 2, ( #9341, #534, #6834, #4604, #2817, #7845, #1974 ),
 .UNSPECIFIED., .F., .F. ) 
 B_SPLINE_CURVE_WITH_KNOTS ( ( 3, 2, 2, 3 ),
 ( 0.9166666666666666297, 0.9444444444444444198, 0.9722222222222222099, 1.000000000000000000 ),
 .UNSPECIFIED. ) 
 CURVE ( )  GEOMETRIC_REPRESENTATION_ITEM ( )  RATIONAL_B_SPLINE_CURVE ( ( 1.000000000000000000, 0.8660254037844387076, 1.000000000000000000, 0.8660254037844387076, 1.000000000000000000, 0.8660254037844387076, 1.000000000000000000 ) ) 
 REPRESENTATION_ITEM ( '' )  );
#7249 = CARTESIAN_POINT ( 'NONE',  ( -0.8603895577212598011, -5.432285873273260179, 1.119999999999999885 ) ) ;
#7250 = LINE ( 'NONE', #9599, #4465 ) ;
#7251 = CARTESIAN_POINT ( 'NONE',  ( -0.9046671180729963790, 5.711843387010016926, 2.379999999999999893 ) ) ;
#7252 = VERTEX_POINT ( 'NONE', #9609 ) ;
#7253 = CARTESIAN_POINT ( 'NONE',  ( 1.500000000000000000, -13.86602540378444459, -1.604166668032260379 ) ) ;
#7254 = EDGE_CURVE ( 'NONE', #1349, #505, #5176, .T. ) ;
#7255 = EDGE_LOOP ( 'NONE', ( #6454, #6617, #2110, #6370 ) ) ;
#7256 = CARTESIAN_POINT ( 'NONE',  ( 8.000000000000001776, 6.100541242131515496, -3.528937025535514138 ) ) ;
#7257 = DIRECTION ( 'NONE',  ( 1.000000000000000000, -0.000000000000000000, -0.000000000000000000 ) ) ;
#7258 = CARTESIAN_POINT ( 'NONE',  ( 0.000000000000000000, 0.000000000000000000, 3.000000000000000000 ) ) ;
#7259 = DIRECTION ( 'NONE',  ( 1.000000000000000000, -0.000000000000000000, -0.000000000000000000 ) ) ;
#7260 = DIRECTION ( 'NONE',  ( 1.000000000000000000, -0.000000000000000000, -0.000000000000000000 ) ) ;
#7261 = CARTESIAN_POINT ( 'NONE',  ( -4.444597532678119300, -0.7039550926810477227, 12.87999999999999901 ) ) ;
#7262 = EDGE_CURVE ( 'NONE', #2426, #5739, #801, .T. ) ;
#7263 = ORIENTED_EDGE ( 'NONE', *, *, #9009, .F. ) ;
#7264 = EDGE_CURVE ( 'NONE', #9050, #8424, #3323, .T. ) ;
#7265 = CIRCLE ( 'NONE', #2866, 6.248999999999999666 ) ;
#7266 = DIRECTION ( 'NONE',  ( -1.000000000000000000, -0.000000000000000000, -0.000000000000000000 ) ) ;
#7267 = CARTESIAN_POINT ( 'NONE',  ( 0.9046671180729951578, -5.711843387010016926, 6.579999999999999183 ) ) ;
#7268 = FACE_OUTER_BOUND ( 'NONE', #5657, .T. ) ;
#7269 = AXIS2_PLACEMENT_3D ( 'NONE', #177, #4401, #5833 ) ;
#7270 = APPLICATION_PROTOCOL_DEFINITION ( 'draft international standard', 'automotive_design', 1998, #10015 ) ;
#7271 = CARTESIAN_POINT ( 'NONE',  ( 3.889087296526005488, 3.889087296526018811, 2.799999999999999378 ) ) ;
#7272 = AXIS2_PLACEMENT_3D ( 'NONE', #10231, #2804, #7684 ) ;
#7273 = DIRECTION ( 'NONE',  ( -0.3420201433256627732, 0.9396926207859105373, 0.000000000000000000 ) ) ;
#7274 = VECTOR ( 'NONE', #8306, 1000.000000000000000 ) ;
#7275 = CARTESIAN_POINT ( 'NONE',  ( 17.58618750323380908, 6.000000000000000000, -12.00000000000000000 ) ) ;
#7276 = CARTESIAN_POINT ( 'NONE',  ( 0.000000000000000000, -4.000000000000000000, -12.00000000000000000 ) ) ;
#7277 = CARTESIAN_POINT ( 'NONE',  ( -2.000000000000000000, -5.522688772756355391, -6.461416928141300531 ) ) ;
#7278 = ADVANCED_FACE ( 'NONE', ( #8909 ), #3130, .F. ) ;
#7279 = CARTESIAN_POINT ( 'NONE',  ( 18.30309047890528618, 12.66178012940252451, 0.000000000000000000 ) ) ;
#7280 = CARTESIAN_POINT ( 'NONE',  ( 14.44459485323380576, 6.000000000000000000, -12.00000000000000000 ) ) ;
#7281 = CARTESIAN_POINT ( 'NONE',  ( 2.231261971483764484, 4.173491630687871101, 4.463948283277976437 ) ) ;
#7282 = UNCERTAINTY_MEASURE_WITH_UNIT (LENGTH_MEASURE( 1.000000000000000082E-05 ), #1906, 'distance_accuracy_value', 'NONE');
#7283 = VECTOR ( 'NONE', #10243, 1000.000000000000000 ) ;
#7284 = CARTESIAN_POINT ( 'NONE',  ( -0.7500000000000007772, -14.29903810567666156, -0.6666666666666669627 ) ) ;
#7285 = ORIENTED_EDGE ( 'NONE', *, *, #9528, .T. ) ;
#7286 = VERTEX_POINT ( 'NONE', #1649 ) ;
#7287 = DIRECTION ( 'NONE',  ( -1.000000000000000000, -0.000000000000000000, -0.000000000000000000 ) ) ;
#7288 = VECTOR ( 'NONE', #8884, 1000.000000000000000 ) ;
#7289 = FACE_OUTER_BOUND ( 'NONE', #10277, .T. ) ;
#7290 = EDGE_LOOP ( 'NONE', ( #9174, #8611, #1811, #8924 ) ) ;
#7291 = ADVANCED_FACE ( 'NONE', ( #5508 ), #8958, .F. ) ;
#7292 = AXIS2_PLACEMENT_3D ( 'NONE', #8971, #758, #10477 ) ;
#7293 = CARTESIAN_POINT ( 'NONE',  ( 2.042957248827968808, -4.009529358847652603, 3.639999999999999680 ) ) ;
#7294 = DIRECTION ( 'NONE',  ( 1.000000000000000000, 0.000000000000000000, -0.000000000000000000 ) ) ;
#7295 = ORIENTED_EDGE ( 'NONE', *, *, #4359, .T. ) ;
#7296 = CARTESIAN_POINT ( 'NONE',  ( 0.7727076532861471003, 5.446173322633805824, 14.71605171672202239 ) ) ;
#7297 = VECTOR ( 'NONE', #7368, 1000.000000000000000 ) ;
#7298 = VECTOR ( 'NONE', #3197, 1000.000000000000000 ) ;
#7299 = ORIENTED_EDGE ( 'NONE', *, *, #9504, .F. ) ;
#7300 = FILL_AREA_STYLE_COLOUR ( '', #10076 ) ;
#7301 = ORIENTED_EDGE ( 'NONE', *, *, #2986, .F. ) ;
#7302 = CIRCLE ( 'NONE', #8655, 2.750000000000000000 ) ;
#7303 = DIRECTION ( 'NONE',  ( -1.000000000000000000, 0.000000000000000000, -0.000000000000000000 ) ) ;
#7304 = CARTESIAN_POINT ( 'NONE',  ( 10.00000000000000000, 0.6700234925293845345, -8.473551116235670477 ) ) ;
#7305 = CIRCLE ( 'NONE', #1376, 8.500000000000000000 ) ;
#7306 = VERTEX_POINT ( 'NONE', #4822 ) ;
#7307 = CARTESIAN_POINT ( 'NONE',  ( 5.152728359536493663, 2.625446233515533745, 8.539999999999999147 ) ) ;
#7308 = CARTESIAN_POINT ( 'NONE',  ( 30.00000000000001066, -34.99999999999999289, 9.000000000000000000 ) ) ;
#7309 = CARTESIAN_POINT ( 'NONE',  ( -2.417848759854264618, 4.940838830814694660, 12.44394828327797597 ) ) ;
#7310 = ORIENTED_EDGE ( 'NONE', *, *, #6326, .F. ) ;
#7311 = CARTESIAN_POINT ( 'NONE',  ( 1.229367062500000385, -12.29022459553277002, -2.677083334016129967 ) ) ;
#7312 = ADVANCED_FACE ( 'NONE', ( #3236, #6403 ), #4931, .F. ) ;
#7313 = SHAPE_REPRESENTATION_RELATIONSHIP ( 'NONE' , 'NONE' ,  #9430, #9288 ) ;
#7314 = ORIENTED_EDGE ( 'NONE', *, *, #2007, .T. ) ;
#7315 = DIRECTION ( 'NONE',  ( -1.000000000000000000, 0.000000000000000000, -0.000000000000000000 ) ) ;
#7316 = EDGE_CURVE ( 'NONE', #2753, #7403, #7150, .T. ) ;
#7317 = FACE_OUTER_BOUND ( 'NONE', #565, .T. ) ;
#7318 = CARTESIAN_POINT ( 'NONE',  ( 0.1499999999999973577, 0.000000000000000000, 0.000000000000000000 ) ) ;
#7319 = DIRECTION ( 'NONE',  ( 1.000000000000000000, 0.000000000000000000, 0.000000000000000000 ) ) ;
#7320 = DIRECTION ( 'NONE',  ( -0.7071067811865465735, -0.7071067811865483499, 0.000000000000000000 ) ) ;
#7321 = CARTESIAN_POINT ( 'NONE',  ( 4.658724279160018966, -0.8323763977770426425, 2.223948283277975779 ) ) ;
#7322 = ORIENTED_EDGE ( 'NONE', *, *, #7743, .T. ) ;
#7323 = CARTESIAN_POINT ( 'NONE',  ( 1.229367062500000163, -13.00000000000000533, -0.3437500006827965970 ) ) ;
#7324 = CARTESIAN_POINT ( 'NONE',  ( -4.900535883036028828, 2.496947748567499126, 4.759999999999999787 ) ) ;
#7325 = DIRECTION ( 'NONE',  ( 1.000000000000000000, 0.000000000000000000, 0.000000000000000000 ) ) ;
#7326 = CONTEXT_DEPENDENT_SHAPE_REPRESENTATION ( #3982, #7679 ) ;
#7327 = CARTESIAN_POINT ( 'NONE',  ( 1.999999999999984013, 35.00000000000000000, -4.000000000000009770 ) ) ;
#7328 = CARTESIAN_POINT ( 'NONE',  ( 20.11292429676619520, 6.000000000000000000, -12.00000000000000000 ) ) ;
#7329 = LINE ( 'NONE', #1661, #4498 ) ;
#7330 = CYLINDRICAL_SURFACE ( 'NONE', #3563, 1.599999999999992983 ) ;
#7331 = PRODUCT ( 'spring', 'spring', '', ( #1443 ) ) ;
#7332 = LINE ( 'NONE', #711, #7445 ) ;
#7333 = CARTESIAN_POINT ( 'NONE',  ( -2.064922774268895811, -4.258245684917318918, 7.856051716722022071 ) ) ;
#7334 =( LENGTH_UNIT ( ) NAMED_UNIT ( * ) SI_UNIT ( .MILLI., .METRE. ) );
#7335 = CARTESIAN_POINT ( 'NONE',  ( 8.000000000000001776, -3.573533178329545645, -5.126388750707257635 ) ) ;
#7336 = CARTESIAN_POINT ( 'NONE',  ( 3.244753828200538148, 3.119207202478391672, 7.403948283277976827 ) ) ;
#7337 = VECTOR ( 'NONE', #8755, 1000.000000000000000 ) ;
#7338 = CARTESIAN_POINT ( 'NONE',  ( 8.692241771943170539E-17, -11.58044919106553650, -2.093750000682796486 ) ) ;
#7339 = ORIENTED_EDGE ( 'NONE', *, *, #10201, .F. ) ;
#7340 = ADVANCED_FACE ( 'NONE', ( #10465 ), #4707, .T. ) ;
#7341 = ADVANCED_FACE ( 'NONE', ( #2393 ), #5614, .F. ) ;
#7342 = ORIENTED_EDGE ( 'NONE', *, *, #7005, .T. ) ;
#7343 = LINE ( 'NONE', #2472, #9171 ) ;
#7344 = AXIS2_PLACEMENT_3D ( 'NONE', #1068, #912, #2455 ) ;
#7345 = CARTESIAN_POINT ( 'NONE',  ( 10.00000000000000000, 52.93638525830372998, 2.343061888689529582 ) ) ;
#7346 = ORIENTED_EDGE ( 'NONE', *, *, #1899, .F. ) ;
#7347 = CARTESIAN_POINT ( 'NONE',  ( 13.82973899676619745, -10.00000000000000000, 0.000000000000000000 ) ) ;
#7348 = CARTESIAN_POINT ( 'NONE',  ( 2.399999999999999911, 2.939152317953647106E-16, -14.00000000000000178 ) ) ;
#7349 = ORIENTED_EDGE ( 'NONE', *, *, #1183, .F. ) ;
#7350 = CARTESIAN_POINT ( 'NONE',  ( 4.173491630687861331, 2.231261971483781359, 6.736051716722023741 ) ) ;
#7351 = VERTEX_POINT ( 'NONE', #1700 ) ;
#7352 = STYLED_ITEM ( 'NONE', ( #998 ), #9288 ) ;
#7353 = EDGE_CURVE ( 'NONE', #6335, #8200, #8284, .T. ) ;
#7354 = APPLICATION_PROTOCOL_DEFINITION ( 'draft international standard', 'automotive_design', 1998, #8858 ) ;
#7355 = VERTEX_POINT ( 'NONE', #2284 ) ;
#7356 = LINE ( 'NONE', #5064, #942 ) ;
#7357 = DIRECTION ( 'NONE',  ( 0.000000000000000000, 0.000000000000000000, -1.000000000000000000 ) ) ;
#7358 = ORIENTED_EDGE ( 'NONE', *, *, #3079, .F. ) ;
#7359 = CARTESIAN_POINT ( 'NONE',  ( 4.089228379062037178, -4.089228379062022967, 3.499999999999998668 ) ) ;
#7360 = CARTESIAN_POINT ( 'NONE',  ( -0.9046671180729963790, 5.711843387010016926, 5.179999999999999716 ) ) ;
#7361 =( GEOMETRIC_REPRESENTATION_CONTEXT ( 3 ) GLOBAL_UNCERTAINTY_ASSIGNED_CONTEXT ( ( #10125 ) ) GLOBAL_UNIT_ASSIGNED_CONTEXT ( ( #6125, #3960, #9483 ) ) REPRESENTATION_CONTEXT ( 'NONE', 'WORKASPACE' ) );
#7362 = CARTESIAN_POINT ( 'NONE',  ( 0.8603895577212593571, 5.432285873273261068, 2.519999999999999574 ) ) ;
#7363 = ORIENTED_EDGE ( 'NONE', *, *, #3498, .T. ) ;
#7364 = CARTESIAN_POINT ( 'NONE',  ( -0.7500000000000007772, -14.29903810567666156, -0.7291666680322601568 ) ) ;
#7365 = AXIS2_PLACEMENT_3D ( 'NONE', #633, #8801, #7902 ) ;
#7366 = ORIENTED_EDGE ( 'NONE', *, *, #4881, .T. ) ;
#7367 = CARTESIAN_POINT ( 'NONE',  ( -2.000000000000012879, 15.00000000000000355, 3.999999999999986233 ) ) ;
#7368 = DIRECTION ( 'NONE',  ( -0.000000000000000000, -0.000000000000000000, -1.000000000000000000 ) ) ;
#7369 = CARTESIAN_POINT ( 'NONE',  ( -2.000000000000000000, -5.349675154362301122, -3.229702268444983648 ) ) ;
#7370 = DIRECTION ( 'NONE',  ( -0.000000000000000000, -0.000000000000000000, 1.000000000000000000 ) ) ;
#7371 = AXIS2_PLACEMENT_3D ( 'NONE', #6070, #9325, #2064 ) ;
#7372 = DIRECTION ( 'NONE',  ( -1.000000000000000000, -0.000000000000000000, -0.000000000000000000 ) ) ;
#7373 = CARTESIAN_POINT ( 'NONE',  ( -4.009529358847660596, 2.042957248827953265, 13.15999999999999837 ) ) ;
#7374 = ORIENTED_EDGE ( 'NONE', *, *, #36, .F. ) ;
#7375 = LINE ( 'NONE', #5564, #9324 ) ;
#7376 = CARTESIAN_POINT ( 'NONE',  ( 4.900535883036028828, -2.496947748567499126, 8.959999999999999076 ) ) ;
#7377 = LINE ( 'NONE', #121, #4622 ) ;
#7378 = AXIS2_PLACEMENT_3D ( 'NONE', #174, #5829, #5878 ) ;
#7379 = CARTESIAN_POINT ( 'NONE',  ( 0.8603895577212593571, 5.432285873273261068, 10.91999999999999993 ) ) ;
#7380 = CIRCLE ( 'NONE', #2812, 3.000000000000000000 ) ;
#7381 = DIRECTION ( 'NONE',  ( -1.000000000000000000, 0.000000000000000000, 0.000000000000000000 ) ) ;
#7382 = DIRECTION ( 'NONE',  ( 0.3420201433256627732, -0.9396926207859105373, 0.000000000000000000 ) ) ;
#7383 = CARTESIAN_POINT ( 'NONE',  ( 10.00000000000000000, -2.652816298622379776, -5.657964889053610946 ) ) ;
#7384 = CARTESIAN_POINT ( 'NONE',  ( 1.300000000000000044, 1.478016689125442484, -1.626303258728256651E-15 ) ) ;
#7385 = CARTESIAN_POINT ( 'NONE',  ( 3.411736077305382420, -3.279728542977940364, 4.496051716722022640 ) ) ;
#7386 = AXIS2_PLACEMENT_3D ( 'NONE', #7800, #536, #9449 ) ;
#7387 = DIRECTION ( 'NONE',  ( 0.000000000000000000, -1.000000000000000000, -0.000000000000000000 ) ) ;
#7388 = VECTOR ( 'NONE', #8959, 1000.000000000000000 ) ;
#7389 = EDGE_CURVE ( 'NONE', #1478, #3324, #7958, .T. ) ;
#7390 = CARTESIAN_POINT ( 'NONE',  ( -2.231261971483764484, -4.173491630687871101, 3.063948283277976081 ) ) ;
#7391 = DIRECTION ( 'NONE',  ( -0.000000000000000000, 1.000000000000000000, -0.000000000000000000 ) ) ;
#7392 = ORIENTED_EDGE ( 'NONE', *, *, #8678, .T. ) ;
#7393 = VERTEX_POINT ( 'NONE', #695 ) ;
#7394 = DIRECTION ( 'NONE',  ( -1.000000000000000000, -0.000000000000000000, -0.000000000000000000 ) ) ;
#7395 = DIRECTION ( 'NONE',  ( -1.156482317317871478E-16, 1.000000000000000000, 0.000000000000000000 ) ) ;
#7396 = ORIENTED_EDGE ( 'NONE', *, *, #9134, .T. ) ;
#7397 = CARTESIAN_POINT ( 'NONE',  ( 3.181980515339458471, 3.181980515339470461, 5.599999999999998757 ) ) ;
#7398 =( NAMED_UNIT ( * ) SI_UNIT ( $, .STERADIAN. ) SOLID_ANGLE_UNIT ( ) );
#7399 = ORIENTED_EDGE ( 'NONE', *, *, #2734, .F. ) ;
#7400 = EDGE_CURVE ( 'NONE', #4726, #1894, #5559, .T. ) ;
#7401 = ADVANCED_FACE ( 'NONE', ( #746 ), #4770, .F. ) ;
#7402 = CARTESIAN_POINT ( 'NONE',  ( -0.6162731882459178134, -4.458484982038665834, 7.716051716722023279 ) ) ;
#7403 = VERTEX_POINT ( 'NONE', #5131 ) ;
#7404 = EDGE_LOOP ( 'NONE', ( #6672, #9721 ) ) ;
#7405 = LINE ( 'NONE', #8315, #2294 ) ;
#7406 = DIRECTION ( 'NONE',  ( -0.000000000000000000, 1.000000000000000000, 0.000000000000000000 ) ) ;
#7407 = ORIENTED_EDGE ( 'NONE', *, *, #10201, .T. ) ;
#7408 = CARTESIAN_POINT ( 'NONE',  ( 2.625446233515515537, 5.152728359536502545, 5.459999999999997300 ) ) ;
#7409 = CARTESIAN_POINT ( 'NONE',  ( 0.8603895577212593571, 5.432285873273261068, 5.319999999999999396 ) ) ;
#7410 = CARTESIAN_POINT ( 'NONE',  ( -2.708615832122950096, -5.110351332421780413, 11.46394828327797555 ) ) ;
#7411 = VERTEX_POINT ( 'NONE', #1960 ) ;
#7412 = EDGE_CURVE ( 'NONE', #1211, #9529, #1014, .T. ) ;
#7413 = CARTESIAN_POINT ( 'NONE',  ( 22.43558391966725907, -7.750000000000000000, 0.000000000000000000 ) ) ;
#7414 = EDGE_LOOP ( 'NONE', ( #2684, #6967, #10456 ) ) ;
#7415 = DIRECTION ( 'NONE',  ( -1.000000000000000000, 0.000000000000000000, -0.000000000000000000 ) ) ;
#7416 = DIRECTION ( 'NONE',  ( 1.000000000000000000, 0.000000000000000000, 0.000000000000000000 ) ) ;
#7417 = DIRECTION ( 'NONE',  ( -1.000000000000000000, 0.000000000000000000, 0.000000000000000000 ) ) ;
#7418 = ORIENTED_EDGE ( 'NONE', *, *, #7662, .T. ) ;
#7419 = DIRECTION ( 'NONE',  ( 0.3420201433256627732, -0.9396926207859105373, 0.000000000000000000 ) ) ;
#7420 = CARTESIAN_POINT ( 'NONE',  ( 0.6146835312499993043, -14.06466310670085562, -0.4270833340161298564 ) ) ;
#7421 = CARTESIAN_POINT ( 'NONE',  ( 2.042957248827968808, -4.009529358847652603, 12.03999999999999915 ) ) ;
#7422 = EDGE_LOOP ( 'NONE', ( #2474, #5795, #3086, #8325 ) ) ;
#7423 = DIRECTION ( 'NONE',  ( 0.000000000000000000, 0.000000000000000000, 1.000000000000000000 ) ) ;
#7424 = CARTESIAN_POINT ( 'NONE',  ( 4.900535883036028828, -2.496947748567499126, 0.5599999999999999423 ) ) ;
#7425 = CARTESIAN_POINT ( 'NONE',  ( 4.404961046766194599, -10.00000000000000000, -12.00000000000000000 ) ) ;
#7426 = ITEM_DEFINED_TRANSFORMATION ( 'NONE', 'NONE', #936,  #2101 ) ;
#7427 = CARTESIAN_POINT ( 'NONE',  ( -4.900535883036028828, 2.496947748567499126, 4.759999999999999787 ) ) ;
#7428 =( REPRESENTATION_RELATIONSHIP ('NONE','NONE', #5100, #1027 ) REPRESENTATION_RELATIONSHIP_WITH_TRANSFORMATION ( #7222 )SHAPE_REPRESENTATION_RELATIONSHIP( ) );
#7429 = LINE ( 'NONE', #4294, #8406 ) ;
#7430 = CARTESIAN_POINT ( 'NONE',  ( -5.999999999999999112, -27.00000000000000711, -17.00000000000000000 ) ) ;
#7431 = VECTOR ( 'NONE', #4801, 1000.000000000000000 ) ;
#7432 = ADVANCED_FACE ( 'NONE', ( #7479 ), #2548, .F. ) ;
#7433 = DIRECTION ( 'NONE',  ( 0.000000000000000000, 0.000000000000000000, 1.000000000000000000 ) ) ;
#7434 = CARTESIAN_POINT ( 'NONE',  ( 4.430710083317573655, 0.7916369971161595354, 4.076051716722022711 ) ) ;
#7435 = DIRECTION ( 'NONE',  ( -1.000000000000000000, -0.000000000000000000, -0.000000000000000000 ) ) ;
#7436 = CARTESIAN_POINT ( 'NONE',  ( -0.7916369971161423269, -4.430710083317576320, 8.523948283277976046 ) ) ;
#7437 = ADVANCED_FACE ( 'NONE', ( #904 ), #8332, .T. ) ;
#7438 = EDGE_CURVE ( 'NONE', #7164, #9442, #2373, .T. ) ;
#7439 = DIRECTION ( 'NONE',  ( -1.000000000000000000, -0.000000000000000000, -0.000000000000000000 ) ) ;
#7440 = AXIS2_PLACEMENT_3D ( 'NONE', #6159, #7168, #6375 ) ;
#7441 = EDGE_LOOP ( 'NONE', ( #6701, #10071, #2723, #1202 ) ) ;
#7442 = AXIS2_PLACEMENT_3D ( 'NONE', #2654, #9223, #7630 ) ;
#7443 = CARTESIAN_POINT ( 'NONE',  ( -0.9046671180729963790, 5.711843387010016926, 13.57999999999999474 ) ) ;
#7444 = CARTESIAN_POINT ( 'NONE',  ( 25.57717656966725883, -7.750000000000000000, 0.000000000000000000 ) ) ;
#7445 = VECTOR ( 'NONE', #3252, 1000.000000000000000 ) ;
#7446 = ADVANCED_FACE ( 'NONE', ( #3391 ), #316, .F. ) ;
#7447 = CARTESIAN_POINT ( 'NONE',  ( 1.300000000000000044, 1.478016689125442484, -1.626303258728256651E-15 ) ) ;
#7448 = ORIENTED_EDGE ( 'NONE', *, *, #4757, .T. ) ;
#7449 = AXIS2_PLACEMENT_3D ( 'NONE', #6448, #624, #6392 ) ;
#7450 = CARTESIAN_POINT ( 'NONE',  ( 4.444597532678119300, 0.7039550926810472786, 0.2799999999999999711 ) ) ;
#7451 = CARTESIAN_POINT ( 'NONE',  ( 1.263368396766194612, 6.000000000000000000, -12.00000000000000000 ) ) ;
#7452 = ORIENTED_EDGE ( 'NONE', *, *, #7264, .F. ) ;
#7453 = CIRCLE ( 'NONE', #8133, 3.000000000000000000 ) ;
#7454 = CARTESIAN_POINT ( 'NONE',  ( -2.122056237541221968, 3.969226411068977889, 6.036051716722022675 ) ) ;
#7455 = LINE ( 'NONE', #200, #4963 ) ;
#7456 = VERTEX_POINT ( 'NONE', #7369 ) ;
#7457 = AXIS2_PLACEMENT_3D ( 'NONE', #7017, #1405, #9637 ) ;
#7458 = ORIENTED_EDGE ( 'NONE', *, *, #3125, .F. ) ;
#7459 = EDGE_CURVE ( 'NONE', #3241, #6828, #9923, .T. ) ;
#7460 = DIRECTION ( 'NONE',  ( 0.000000000000000000, 0.000000000000000000, 1.000000000000000000 ) ) ;
#7461 = VECTOR ( 'NONE', #1235, 1000.000000000000000 ) ;
#7462 = MECHANICAL_DESIGN_GEOMETRIC_PRESENTATION_REPRESENTATION (  '', ( #8647 ), #3566 ) ;
#7463 = CARTESIAN_POINT ( 'NONE',  ( 1.060575238724907038E-16, -11.26794919243112680, -0.3750000000000002776 ) ) ;
#7464 = EDGE_LOOP ( 'NONE', ( #4269, #2387, #3916, #3310 ) ) ;
#7465 = CARTESIAN_POINT ( 'NONE',  ( -5.432285873273256627, -0.8603895577212797852, 10.07999999999999829 ) ) ;
#7466 = CARTESIAN_POINT ( 'NONE',  ( -5.432285873273256627, -0.8603895577212797852, 4.479999999999999538 ) ) ;
#7467 = VECTOR ( 'NONE', #8707, 1000.000000000000000 ) ;
#7468 = CARTESIAN_POINT ( 'NONE',  ( 4.900535883036028828, -2.496947748567499126, 0.5599999999999999423 ) ) ;
#7469 = ORIENTED_EDGE ( 'NONE', *, *, #4976, .T. ) ;
#7470 = VECTOR ( 'NONE', #7655, 1000.000000000000114 ) ;
#7471 = CARTESIAN_POINT ( 'NONE',  ( 1.229367062500000163, -13.00000000000000533, -1.218750000682796486 ) ) ;
#7472 = AXIS2_PLACEMENT_3D ( 'NONE', #6332, #3162, #1524 ) ;
#7473 = ORIENTED_EDGE ( 'NONE', *, *, #6616, .F. ) ;
#7474 = AXIS2_PLACEMENT_3D ( 'NONE', #8198, #7394, #4157 ) ;
#7475 = EDGE_CURVE ( 'NONE', #10281, #8011, #8303, .T. ) ;
#7476 = FACE_OUTER_BOUND ( 'NONE', #7973, .T. ) ;
#7477 = EDGE_CURVE ( 'NONE', #9713, #1643, #1060, .T. ) ;
#7478 = CARTESIAN_POINT ( 'NONE',  ( -29.99999999999998934, -13.00000000000000533, 1.249999999999987121 ) ) ;
#7479 = FACE_OUTER_BOUND ( 'NONE', #2319, .T. ) ;
#7480 = ORIENTED_EDGE ( 'NONE', *, *, #9463, .T. ) ;
#7481 = DIRECTION ( 'NONE',  ( -1.000000000000000000, -0.000000000000000000, -0.000000000000000000 ) ) ;
#7482 = CARTESIAN_POINT ( 'NONE',  ( -0.6146835312500006365, -14.06466310670085562, -2.010416667349463005 ) ) ;
#7483 = CARTESIAN_POINT ( 'NONE',  ( 3.244753828200538148, 3.119207202478391672, 1.803948283277976516 ) ) ;
#7484 = ORIENTED_EDGE ( 'NONE', *, *, #1057, .F. ) ;
#7485 = FACE_OUTER_BOUND ( 'NONE', #3011, .T. ) ;
#7486 = CARTESIAN_POINT ( 'NONE',  ( 4.089228379062037178, -4.089228379062022967, 3.499999999999998668 ) ) ;
#7487 = DIRECTION ( 'NONE',  ( 0.000000000000000000, 0.000000000000000000, 1.000000000000000000 ) ) ;
#7488 = EDGE_CURVE ( 'NONE', #48, #6283, #5965, .T. ) ;
#7489 = CARTESIAN_POINT ( 'NONE',  ( -5.432285873273256627, -0.8603895577212797852, 4.479999999999999538 ) ) ;
#7490 = CYLINDRICAL_SURFACE ( 'NONE', #10097, 6.248999999999999666 ) ;
#7491 = DIRECTION ( 'NONE',  ( 1.000000000000000000, 0.000000000000000000, 0.000000000000000000 ) ) ;
#7492 = PLANE ( 'NONE',  #3544 ) ;
#7493 = CARTESIAN_POINT ( 'NONE',  ( 3.411736077305382420, -3.279728542977940364, 7.296051716722023350 ) ) ;
#7494 = CARTESIAN_POINT ( 'NONE',  ( -0.6146835312500006365, -14.06466310670085562, -1.385416667349463227 ) ) ;
#7495 = CARTESIAN_POINT ( 'NONE',  ( -0.6479879772514802738, 4.687928535947285091, 6.983948283277976010 ) ) ;
#7496 = CARTESIAN_POINT ( 'NONE',  ( -17.00000000000000000, 19.99999999999999645, 6.000000000000000000 ) ) ;
#7497 = ORIENTED_EDGE ( 'NONE', *, *, #6933, .F. ) ;
#7498 = CARTESIAN_POINT ( 'NONE',  ( 0.7727076532861471003, 5.446173322633805824, 3.516051716722023102 ) ) ;
#7499 = CARTESIAN_POINT ( 'NONE',  ( 16.98057649071655817, -10.02539999999999942, -12.00000000000000000 ) ) ;
#7500 = CARTESIAN_POINT ( 'NONE',  ( 8.000000000000001776, 4.137773741518453008, -5.705158055754754542 ) ) ;
#7501 = EDGE_CURVE ( 'NONE', #10421, #4827, #6839, .T. ) ;
#7502 = ORIENTED_EDGE ( 'NONE', *, *, #353, .T. ) ;
#7503 = CARTESIAN_POINT ( 'NONE',  ( 3.181980515339458471, 3.181980515339470461, 11.19999999999999751 ) ) ;
#7504 = VECTOR ( 'NONE', #681, 1000.000000000000000 ) ;
#7505 = PRESENTATION_STYLE_ASSIGNMENT (( #4259 ) ) ;
#7506 = ORIENTED_EDGE ( 'NONE', *, *, #2607, .T. ) ;
#7507 = CARTESIAN_POINT ( 'NONE',  ( -4.430710083317573655, -0.7916369971161599794, 8.276051716722021112 ) ) ;
#7508 = CARTESIAN_POINT ( 'NONE',  ( 0.6146835312500001924, -11.93533689329915326, -2.260416667349463449 ) ) ;
#7509 = EDGE_CURVE ( 'NONE', #10163, #244, #8277, .T. ) ;
#7510 = VERTEX_POINT ( 'NONE', #3541 ) ;
#7511 = CARTESIAN_POINT ( 'NONE',  ( -1.836970198721025743E-16, 0.000000000000000000, 32.99999999999998579 ) ) ;
#7512 = ORIENTED_EDGE ( 'NONE', *, *, #2543, .F. ) ;
#7513 = AXIS2_PLACEMENT_3D ( 'NONE', #9444, #742, #7843 ) ;
#7514 = DIRECTION ( 'NONE',  ( -1.000000000000000000, -0.000000000000000000, -0.000000000000000000 ) ) ;
#7515 = ORIENTED_EDGE ( 'NONE', *, *, #7866, .T. ) ;
#7516 = CARTESIAN_POINT ( 'NONE',  ( 5.418398423912711870, 0.9480714621563913758, 1.276051716722023333 ) ) ;
#7517 = CARTESIAN_POINT ( 'NONE',  ( -4.089228379062038066, 4.089228379062021190, 2.099999999999999201 ) ) ;
#7518 = CARTESIAN_POINT ( 'NONE',  ( 3.889087296526005488, 3.889087296526018811, 8.400000000000000355 ) ) ;
#7519 = ORIENTED_EDGE ( 'NONE', *, *, #1377, .F. ) ;
#7520 = CARTESIAN_POINT ( 'NONE',  ( -1.229367062500000163, -13.00000000000000533, 0.03124999931720332663 ) ) ;
#7521 = ADVANCED_FACE ( 'NONE', ( #4282 ), #8224, .F. ) ;
#7522 = EDGE_LOOP ( 'NONE', ( #7891, #3567, #4229, #1180 ) ) ;
#7523 = LINE ( 'NONE', #9870, #6843 ) ;
#7524 = DIRECTION ( 'NONE',  ( -1.000000000000000000, -0.000000000000000000, -0.000000000000000000 ) ) ;
#7525 = ORIENTED_EDGE ( 'NONE', *, *, #8186, .T. ) ;
#7526 = LINE ( 'NONE', #8432, #1689 ) ;
#7527 = CARTESIAN_POINT ( 'NONE',  ( 0.6146835312500001924, -11.93533689329915326, -1.760416667349463449 ) ) ;
#7528 = CARTESIAN_POINT ( 'NONE',  ( -4.658724279160018078, 0.8323763977770419764, 9.223948283277977112 ) ) ;
#7529 = ORIENTED_EDGE ( 'NONE', *, *, #6778, .F. ) ;
#7530 = CARTESIAN_POINT ( 'NONE',  ( 5.019816903233806471, -10.00000000000000000, -12.00000000000000000 ) ) ;
#7531 = EDGE_CURVE ( 'NONE', #1639, #7636, #268, .T. ) ;
#7532 = EDGE_CURVE ( 'NONE', #7882, #2911, #5079, .T. ) ;
#7533 = ADVANCED_FACE ( 'NONE', ( #6565 ), #1909, .F. ) ;
#7534 = LINE ( 'NONE', #9181, #1770 ) ;
#7535 = CARTESIAN_POINT ( 'NONE',  ( 7.546553696766195252, 6.000000000000000000, -12.00000000000000000 ) ) ;
#7536 = CARTESIAN_POINT ( 'NONE',  ( -5.152728359536494551, -2.625446233515535521, 9.939999999999997726 ) ) ;
#7537 = AXIS2_PLACEMENT_3D ( 'NONE', #5709, #4181, #8222 ) ;
#7538 = CARTESIAN_POINT ( 'NONE',  ( 1.300000000000000044, -0.7390083445627225744, -1.279999999999999138 ) ) ;
#7539 = CARTESIAN_POINT ( 'NONE',  ( 0.7500000000000003331, -11.70096189432334732, -1.979166668032260157 ) ) ;
#7540 = COLOUR_RGB ( '', 0.66274510, 0.83137255, 0.94901961) ;
#7541 = CARTESIAN_POINT ( 'NONE',  ( 0.000000000000000000, 0.000000000000000000, -12.00000000000000000 ) ) ;
#7542 = CARTESIAN_POINT ( 'NONE',  ( 0.8323763977770604061, -4.658724279160015413, 7.576051716722023599 ) ) ;
#7543 = CARTESIAN_POINT ( 'NONE',  ( 8.692241771943169307E-17, -11.58044919106553294, -1.593750000682796486 ) ) ;
#7544 = ADVANCED_FACE ( 'NONE', ( #2010 ), #5289, .F. ) ;
#7545 = AXIS2_PLACEMENT_3D ( 'NONE', #3064, #8055, #4017 ) ;
#7546 = CARTESIAN_POINT ( 'NONE',  ( -3.951860609387083834, -3.826313983664940466, 0.4039482832779765498 ) ) ;
#7547 = CARTESIAN_POINT ( 'NONE',  ( 1.229367062500000163, -12.29022459553277002, -2.177083334016129523 ) ) ;
#7548 = AXIS2_PLACEMENT_3D ( 'NONE', #1447, #9571, #4673 ) ;
#7549 = EDGE_LOOP ( 'NONE', ( #3530, #6380, #5504, #6204 ) ) ;
#7550 = CARTESIAN_POINT ( 'NONE',  ( 0.9968613283357860011, -5.697241258616382531, 7.576051716722023599 ) ) ;
#7551 = CARTESIAN_POINT ( 'NONE',  ( 1.300000000000000044, -0.7390083445627200209, 1.280000000000001137 ) ) ;
#7552 = VECTOR ( 'NONE', #9237, 1000.000000000000000 ) ;
#7553 = FACE_OUTER_BOUND ( 'NONE', #4696, .T. ) ;
#7554 = ORIENTED_EDGE ( 'NONE', *, *, #1450, .F. ) ;
#7555 = VECTOR ( 'NONE', #5560, 1000.000000000000000 ) ;
#7556 = CARTESIAN_POINT ( 'NONE',  ( 3.181980515339458471, 3.181980515339470461, 8.400000000000000355 ) ) ;
#7557 = CARTESIAN_POINT ( 'NONE',  ( -2.122056237541221968, 3.969226411068977889, 8.836051716722023386 ) ) ;
#7558 = CARTESIAN_POINT ( 'NONE',  ( -2.000000000000000000, -7.673322273190750664, 3.656518192455050276 ) ) ;
#7559 = EDGE_LOOP ( 'NONE', ( #2521, #8746 ) ) ;
#7560 = DIRECTION ( 'NONE',  ( 1.000000000000000000, 0.000000000000000000, 0.000000000000000000 ) ) ;
#7561 = ORIENTED_EDGE ( 'NONE', *, *, #9280, .T. ) ;
#7562 = CARTESIAN_POINT ( 'NONE',  ( -15.00000000000000000, 19.99999999999999645, -5.999999999999999112 ) ) ;
#7563 = FACE_OUTER_BOUND ( 'NONE', #805, .T. ) ;
#7564 = VERTEX_POINT ( 'NONE', #7030 ) ;
#7565 = CARTESIAN_POINT ( 'NONE',  ( 4.940838830814703542, -2.417848759854246410, 4.356051716722023848 ) ) ;
#7566 = CARTESIAN_POINT ( 'NONE',  ( 5.152728359536493663, 2.625446233515533745, 0.1399999999999999856 ) ) ;
#7567 = CARTESIAN_POINT ( 'NONE',  ( 0.8603895577212593571, 5.432285873273261068, 10.91999999999999993 ) ) ;
#7568 = ORIENTED_EDGE ( 'NONE', *, *, #6566, .F. ) ;
#7569 = CARTESIAN_POINT ( 'NONE',  ( -1.229367062500000163, -12.29022459553277002, -1.510416667349463227 ) ) ;
#7570 = ORIENTED_EDGE ( 'NONE', *, *, #9190, .F. ) ;
#7571 = CARTESIAN_POINT ( 'NONE',  ( 1.500000000000000222, -13.00000000000000533, -3.000000000000000000 ) ) ;
#7572 = CARTESIAN_POINT ( 'NONE',  ( -0.7499999999999997780, -11.70096189432334555, -0.8958333346989268975 ) ) ;
#7573 = EDGE_LOOP ( 'NONE', ( #6310, #5597, #7938, #7615 ) ) ;
#7574 = CARTESIAN_POINT ( 'NONE',  ( 10.00000000000000000, -5.848742439617878652, -6.167836887841048110 ) ) ;
#7575 = ADVANCED_FACE ( 'NONE', ( #4592 ), #3748, .F. ) ;
#7576 = DIRECTION ( 'NONE',  ( 0.000000000000000000, 0.000000000000000000, -1.000000000000000000 ) ) ;
#7577 = CARTESIAN_POINT ( 'NONE',  ( 0.6146835312500001924, -11.93533689329915326, -0.2604166673494633377 ) ) ;
#7578 = CARTESIAN_POINT ( 'NONE',  ( 2.231261971483764484, 4.173491630687871101, 12.86394828327797768 ) ) ;
#7579 = EDGE_LOOP ( 'NONE', ( #1196, #5660 ) ) ;
#7580 = FACE_OUTER_BOUND ( 'NONE', #10101, .T. ) ;
#7581 = CARTESIAN_POINT ( 'NONE',  ( -0.9046671180729963790, 5.711843387010016926, 10.77999999999999936 ) ) ;
#7582 = LINE ( 'NONE', #8390, #2448 ) ;
#7583 = CARTESIAN_POINT ( 'NONE',  ( 0.9046671180729953798, -5.711843387010016926, 6.579999999999999183 ) ) ;
#7584 = CARTESIAN_POINT ( 'NONE',  ( 1.300000000000000044, -1.478016689125442706, 1.843143693225357538E-15 ) ) ;
#7585 = ADVANCED_FACE ( 'NONE', ( #4538 ), #2065, .T. ) ;
#7586 = DIRECTION ( 'NONE',  ( -0.000000000000000000, 1.000000000000000000, 0.000000000000000000 ) ) ;
#7587 = ADVANCED_FACE ( 'NONE', ( #1213 ), #10333, .F. ) ;
#7588 = DIRECTION ( 'NONE',  ( 0.000000000000000000, 0.000000000000000000, 1.000000000000000000 ) ) ;
#7589 = CARTESIAN_POINT ( 'NONE',  ( 4.687928535947288644, -0.6479879772514620662, 9.816051716722022036 ) ) ;
#7590 =( BOUNDED_SURFACE ( )  B_SPLINE_SURFACE ( 1, 2, ( 
 ( #8538, #10137, #10238, #2172, #9496, #3701, #3073, #2858, #9336, #10289, #2072, #8636, #2917, #2228, #8688, #1424, #3860, #7088, #10345, #6292, #9548, #3174, #4701, #7253, #9602, #4921, #8950, #3972, #1644, #8168, #898, #6399, #3122, #9655, #6455, #4124, #8904, #2492, #7947, #10402, #4866, #9712, #8852, #10498, #7364, #4024, #8111, #3282, #106, #794, #2383, #3226, #740, #5704, #7201, #844, #5609, #3334, #1594, #9763, #2439, #8008, #685, #53, #4817, #5659, #4075, #3918, #1695, #6349, #5501, #1538, #8063 ),
 ( #10457, #7311, #6505, #2330, #6559, #9811, #8743, #1479, #7143, #5552, #8795, #4765, #366, #3385, #5124, #6613, #2692, #2749, #4227, #6816, #5911, #9168, #9867, #9214, #1800, #4177, #6711, #1101, #3536, #7569, #1054, #5073, #8372, #263, #6761, #8327, #7471, #5177, #5809, #2595, #9917, #9062, #1954, #9113, #9008, #6659, #5960, #2541, #1905, #5760, #5027, #8271, #997, #3590, #9969, #2646, #4972, #212, #4326, #10024, #3436, #1745, #4275, #312, #5861, #1849, #7520, #8425, #3490, #1151, #4375, #7621, #8218 ) ),
 .UNSPECIFIED., .F., .F., .F. ) 
 B_SPLINE_SURFACE_WITH_KNOTS ( ( 2, 2 ),
 ( 3, 2, 2, 2, 2, 2, 2, 2, 2, 2, 2, 2, 2, 2, 2, 2, 2, 2, 2, 2, 2, 2, 2, 2, 2, 2, 2, 2, 2, 2, 2, 2, 2, 2, 2, 2, 3 ),
 ( 0.000000000000000000, 1.000000000000000000 ),
 ( 0.000000000000000000, 0.02777777777777777624, 0.05555555555555555247, 0.08333333333333332871, 0.1111111111111111049, 0.1388888888888888951, 0.1666666666666666574, 0.1944444444444444475, 0.2222222222222222099, 0.2500000000000000000, 0.2777777777777777901, 0.3055555555555555802, 0.3333333333333333148, 0.3611111111111111049, 0.3888888888888888951, 0.4166666666666666852, 0.4444444444444444198, 0.4722222222222222099, 0.5000000000000000000, 0.5277777777777777901, 0.5555555555555555802, 0.5833333333333333703, 0.6111111111111111605, 0.6388888888888888395, 0.6666666666666666297, 0.6944444444444444198, 0.7222222222222222099, 0.7500000000000000000, 0.7777777777777777901, 0.8055555555555555802, 0.8333333333333333703, 0.8611111111111111605, 0.8888888888888888395, 0.9166666666666666297, 0.9444444444444444198, 0.9722222222222222099, 1.000000000000000000 ),
 .UNSPECIFIED. ) 
 GEOMETRIC_REPRESENTATION_ITEM ( )  RATIONAL_B_SPLINE_SURFACE ( (
 ( 1.000000000000000000, 0.8660254037844387076, 1.000000000000000000, 0.8660254037844387076, 1.000000000000000000, 0.8660254037844387076, 1.000000000000000000, 0.8660254037844387076, 1.000000000000000000, 0.8660254037844387076, 1.000000000000000000, 0.8660254037844387076, 1.000000000000000000, 0.8660254037844387076, 1.000000000000000000, 0.8660254037844387076, 1.000000000000000000, 0.8660254037844387076, 1.000000000000000000, 0.8660254037844387076, 1.000000000000000000, 0.8660254037844387076, 1.000000000000000000, 0.8660254037844387076, 1.000000000000000000, 0.8660254037844387076, 1.000000000000000000, 0.8660254037844387076, 1.000000000000000000, 0.8660254037844387076, 1.000000000000000000, 0.8660254037844387076, 1.000000000000000000, 0.8660254037844387076, 1.000000000000000000, 0.8660254037844387076, 1.000000000000000000, 0.8660254037844387076, 1.000000000000000000, 0.8660254037844387076, 1.000000000000000000, 0.8660254037844387076, 1.000000000000000000, 0.8660254037844387076, 1.000000000000000000, 0.8660254037844387076, 1.000000000000000000, 0.8660254037844387076, 1.000000000000000000, 0.8660254037844387076, 1.000000000000000000, 0.8660254037844387076, 1.000000000000000000, 0.8660254037844387076, 1.000000000000000000, 0.8660254037844387076, 1.000000000000000000, 0.8660254037844387076, 1.000000000000000000, 0.8660254037844387076, 1.000000000000000000, 0.8660254037844387076, 1.000000000000000000, 0.8660254037844387076, 1.000000000000000000, 0.8660254037844387076, 1.000000000000000000, 0.8660254037844387076, 1.000000000000000000, 0.8660254037844387076, 1.000000000000000000, 0.8660254037844387076, 1.000000000000000000),
 ( 1.000000000000000000, 0.8660254037844387076, 1.000000000000000000, 0.8660254037844387076, 1.000000000000000000, 0.8660254037844387076, 1.000000000000000000, 0.8660254037844387076, 1.000000000000000000, 0.8660254037844387076, 1.000000000000000000, 0.8660254037844387076, 1.000000000000000000, 0.8660254037844387076, 1.000000000000000000, 0.8660254037844387076, 1.000000000000000000, 0.8660254037844387076, 1.000000000000000000, 0.8660254037844387076, 1.000000000000000000, 0.8660254037844387076, 1.000000000000000000, 0.8660254037844387076, 1.000000000000000000, 0.8660254037844387076, 1.000000000000000000, 0.8660254037844387076, 1.000000000000000000, 0.8660254037844387076, 1.000000000000000000, 0.8660254037844387076, 1.000000000000000000, 0.8660254037844387076, 1.000000000000000000, 0.8660254037844387076, 1.000000000000000000, 0.8660254037844387076, 1.000000000000000000, 0.8660254037844387076, 1.000000000000000000, 0.8660254037844387076, 1.000000000000000000, 0.8660254037844387076, 1.000000000000000000, 0.8660254037844387076, 1.000000000000000000, 0.8660254037844387076, 1.000000000000000000, 0.8660254037844387076, 1.000000000000000000, 0.8660254037844387076, 1.000000000000000000, 0.8660254037844387076, 1.000000000000000000, 0.8660254037844387076, 1.000000000000000000, 0.8660254037844387076, 1.000000000000000000, 0.8660254037844387076, 1.000000000000000000, 0.8660254037844387076, 1.000000000000000000, 0.8660254037844387076, 1.000000000000000000, 0.8660254037844387076, 1.000000000000000000, 0.8660254037844387076, 1.000000000000000000, 0.8660254037844387076, 1.000000000000000000, 0.8660254037844387076, 1.000000000000000000) ) ) 
 REPRESENTATION_ITEM ( '' )  SURFACE ( )  );
#7591 = CARTESIAN_POINT ( 'NONE',  ( -0.6146835312499998594, -11.93533689329915326, -1.052083334016129967 ) ) ;
#7592 = CARTESIAN_POINT ( 'NONE',  ( 4.860232935257354114, -2.576046737280751842, -0.4360517167220233636 ) ) ;
#7593 = CARTESIAN_POINT ( 'NONE',  ( 1.229367062500000163, -13.00000000000000533, -1.218750000682796486 ) ) ;
#7594 = VERTEX_POINT ( 'NONE', #369 ) ;
#7595 = CARTESIAN_POINT ( 'NONE',  ( 5.726445515403654873, -0.8124729078101852187, 7.016051716722022213 ) ) ;
#7596 = AXIS2_PLACEMENT_3D ( 'NONE', #4660, #1434, #7906 ) ;
#7597 = ADVANCED_FACE ( 'NONE', ( #4382 ), #10283, .T. ) ;
#7598 = CARTESIAN_POINT ( 'NONE',  ( 10.00000000000000000, -4.724769925181144359, -4.089810527897808079 ) ) ;
#7599 = DIRECTION ( 'NONE',  ( 0.000000000000000000, -0.000000000000000000, 1.000000000000000000 ) ) ;
#7600 = ORIENTED_EDGE ( 'NONE', *, *, #1047, .T. ) ;
#7601 = CARTESIAN_POINT ( 'NONE',  ( 3.345732310141667387, -3.345732310141654064, 6.299999999999998934 ) ) ;
#7602 = DIRECTION ( 'NONE',  ( 0.000000000000000000, 0.000000000000000000, 1.000000000000000000 ) ) ;
#7603 = VECTOR ( 'NONE', #10212, 1000.000000000000000 ) ;
#7604 = CARTESIAN_POINT ( 'NONE',  ( 0.7039550926810297371, 4.444597532678122853, 2.519999999999999574 ) ) ;
#7605 = CIRCLE ( 'NONE', #2028, 8.500000000000000000 ) ;
#7606 = CARTESIAN_POINT ( 'NONE',  ( -1.229367062500000163, -13.00000000000000533, -0.09375000068279679133 ) ) ;
#7607 = VERTEX_POINT ( 'NONE', #4490 ) ;
#7608 = SHAPE_REPRESENTATION ( 'spring', ( #2101 ), #9398 ) ;
#7609 = CLOSED_SHELL ( 'NONE', ( #5017, #736, #340, #7587, #856, #7063, #7312, #2464, #1363, #2291, #7913, #1232, #1117, #5276, #3321, #7291 ) ) ;
#7610 = ORIENTED_EDGE ( 'NONE', *, *, #5201, .T. ) ;
#7611 = EDGE_CURVE ( 'NONE', #5208, #8384, #7613, .T. ) ;
#7612 = CYLINDRICAL_SURFACE ( 'NONE', #4656, 1.999999999999997780 ) ;
#7613 = CIRCLE ( 'NONE', #1868, 1.280000000000000027 ) ;
#7614 = DIRECTION ( 'NONE',  ( -1.000000000000000000, -0.000000000000000000, -0.000000000000000000 ) ) ;
#7615 = ORIENTED_EDGE ( 'NONE', *, *, #8845, .T. ) ;
#7616 = MECHANICAL_DESIGN_GEOMETRIC_PRESENTATION_REPRESENTATION (  '', ( #5579 ), #4906 ) ;
#7617 = CARTESIAN_POINT ( 'NONE',  ( 4.940838830814703542, -2.417848759854246410, 1.556051716722023581 ) ) ;
#7618 = CARTESIAN_POINT ( 'NONE',  ( 0.9046671180729951578, -5.711843387010016926, 12.17999999999999439 ) ) ;
#7619 = CARTESIAN_POINT ( 'NONE',  ( -2.496947748567517333, 4.900535883036019058, 13.43999999999999950 ) ) ;
#7620 = ORIENTED_EDGE ( 'NONE', *, *, #1835, .F. ) ;
#7621 = CARTESIAN_POINT ( 'NONE',  ( 1.229367062499999719, -13.70977540446724063, 0.2395833326505366900 ) ) ;
#7622 = VECTOR ( 'NONE', #4581, 999.9999999999998863 ) ;
#7623 =( NAMED_UNIT ( * ) PLANE_ANGLE_UNIT ( ) SI_UNIT ( $, .RADIAN. ) );
#7624 = AXIS2_PLACEMENT_3D ( 'NONE', #4841, #1507, #7980 ) ;
#7625 = ORIENTED_EDGE ( 'NONE', *, *, #9970, .T. ) ;
#7626 = EDGE_CURVE ( 'NONE', #317, #2753, #3695, .T. ) ;
#7627 = DIRECTION ( 'NONE',  ( 0.000000000000000000, 0.000000000000000000, 1.000000000000000000 ) ) ;
#7628 = CARTESIAN_POINT ( 'NONE',  ( 13.01080596966725622, 3.750000000000000000, -12.00000000000000000 ) ) ;
#7629 = ORIENTED_EDGE ( 'NONE', *, *, #1437, .T. ) ;
#7630 = DIRECTION ( 'NONE',  ( 0.000000000000000000, 0.000000000000000000, -1.000000000000000000 ) ) ;
#7631 = VECTOR ( 'NONE', #9042, 1000.000000000000000 ) ;
#7632 = DIRECTION ( 'NONE',  ( -1.000000000000000000, -0.000000000000000000, -0.000000000000000000 ) ) ;
#7633 = CARTESIAN_POINT ( 'NONE',  ( 8.692241771943170539E-17, -11.58044919106553650, -1.218750000682796930 ) ) ;
#7634 = EDGE_CURVE ( 'NONE', #10224, #2333, #518, .T. ) ;
#7635 = CARTESIAN_POINT ( 'NONE',  ( 4.258245684917310037, 2.064922774268912686, 10.34394828327797633 ) ) ;
#7636 = VERTEX_POINT ( 'NONE', #6978 ) ;
#7637 = DIRECTION ( 'NONE',  ( -1.000000000000000000, 0.000000000000000000, 0.000000000000000000 ) ) ;
#7638 = AXIS2_PLACEMENT_3D ( 'NONE', #5924, #7423, #276 ) ;
#7639 = CARTESIAN_POINT ( 'NONE',  ( 0.8603895577212593571, 5.432285873273261068, 13.71999999999999886 ) ) ;
#7640 = VECTOR ( 'NONE', #7110, 1000.000000000000000 ) ;
#7641 = LINE ( 'NONE', #379, #6495 ) ;
#7642 = AXIS2_PLACEMENT_3D ( 'NONE', #1612, #8433, #1964 ) ;
#7643 = EDGE_CURVE ( 'NONE', #4426, #4307, #8430, .T. ) ;
#7644 = CARTESIAN_POINT ( 'NONE',  ( -5.152728359536494551, -2.625446233515535521, 12.73999999999999844 ) ) ;
#7645 = CARTESIAN_POINT ( 'NONE',  ( 0.000000000000000000, 0.000000000000000000, 3.000000000000000000 ) ) ;
#7646 = CARTESIAN_POINT ( 'NONE',  ( 1.500000000000000222, -13.00000000000000533, -2.062500001365593416 ) ) ;
#7647 = CARTESIAN_POINT ( 'NONE',  ( 9.869213319667256457, -7.750000000000000000, -12.00000000000000000 ) ) ;
#7648 = CARTESIAN_POINT ( 'NONE',  ( -3.119207202478379681, -3.244753828200550139, 10.79605171672202246 ) ) ;
#7649 = CARTESIAN_POINT ( 'NONE',  ( 1.229367062499999719, -13.70977540446724063, -1.760416667349463227 ) ) ;
#7650 = CARTESIAN_POINT ( 'NONE',  ( -2.708615832122950096, -5.110351332421780413, 0.2639482832779765920 ) ) ;
#7651 = CARTESIAN_POINT ( 'NONE',  ( -2.607672531582950546E-16, -14.41955080893447416, 0.1562499993172034307 ) ) ;
#7652 = ORIENTED_EDGE ( 'NONE', *, *, #9365, .F. ) ;
#7653 = CARTESIAN_POINT ( 'NONE',  ( 2.697157280332745266, -7.750000000000000000, -12.00000000000000000 ) ) ;
#7654 = DIRECTION ( 'NONE',  ( 0.000000000000000000, 0.000000000000000000, 1.000000000000000000 ) ) ;
#7655 = DIRECTION ( 'NONE',  ( 0.000000000000000000, -0.5000000000000009992, -0.8660254037844380415 ) ) ;
#7656 = ORIENTED_EDGE ( 'NONE', *, *, #3375, .F. ) ;
#7657 = CARTESIAN_POINT ( 'NONE',  ( 2.148092372876330369, 4.215868657802594122, 11.05999999999999872 ) ) ;
#7658 = CARTESIAN_POINT ( 'NONE',  ( -13.00000000000000000, 19.99999999999999645, 9.000000000000000000 ) ) ;
#7659 = CARTESIAN_POINT ( 'NONE',  ( 3.345732310141667387, -3.345732310141653620, 3.499999999999998668 ) ) ;
#7660 = ADVANCED_FACE ( 'NONE', ( #471 ), #10077, .F. ) ;
#7661 = CARTESIAN_POINT ( 'NONE',  ( -1.229367062500000385, -13.70977540446723886, -1.052083334016129967 ) ) ;
#7662 = EDGE_CURVE ( 'NONE', #5138, #8250, #1179, .T. ) ;
#7663 = ORIENTED_EDGE ( 'NONE', *, *, #828, .T. ) ;
#7664 = EDGE_CURVE ( 'NONE', #717, #2729, #10130, .T. ) ;
#7665 = SHAPE_REPRESENTATION_RELATIONSHIP ( 'NONE' , 'NONE' ,  #7207, #9161 ) ;
#7666 = ORIENTED_EDGE ( 'NONE', *, *, #996, .T. ) ;
#7667 = DIRECTION ( 'NONE',  ( 0.000000000000000000, -0.000000000000000000, 1.000000000000000000 ) ) ;
#7668 = DIRECTION ( 'NONE',  ( -1.000000000000000000, 0.000000000000000000, 0.000000000000000000 ) ) ;
#7669 = AXIS2_PLACEMENT_3D ( 'NONE', #4813, #8849, #3070 ) ;
#7670 = FACE_OUTER_BOUND ( 'NONE', #3127, .T. ) ;
#7671 = EDGE_LOOP ( 'NONE', ( #10405, #9222, #5216, #9580 ) ) ;
#7672 = CARTESIAN_POINT ( 'NONE',  ( 2.576046737280769605, -4.860232935257343456, 1.836051716722023386 ) ) ;
#7673 = CARTESIAN_POINT ( 'NONE',  ( -4.900535883036028828, 2.496947748567499126, 13.15999999999999837 ) ) ;
#7674 = CARTESIAN_POINT ( 'NONE',  ( 0.8603895577212593571, 5.432285873273261068, 5.319999999999999396 ) ) ;
#7675 = VERTEX_POINT ( 'NONE', #2961 ) ;
#7676 = DIRECTION ( 'NONE',  ( -1.000000000000000000, -0.000000000000000000, -0.000000000000000000 ) ) ;
#7677 = UNCERTAINTY_MEASURE_WITH_UNIT (LENGTH_MEASURE( 1.000000000000000082E-05 ), #8562, 'distance_accuracy_value', 'NONE');
#7678 = EDGE_CURVE ( 'NONE', #2213, #6101, #6128, .T. ) ;
#7679 = PRODUCT_DEFINITION_SHAPE ( 'NONE', 'NONE',  #10509 ) ;
#7680 = VECTOR ( 'NONE', #3137, 1000.000000000000000 ) ;
#7681 =( NAMED_UNIT ( * ) PLANE_ANGLE_UNIT ( ) SI_UNIT ( $, .RADIAN. ) );
#7682 = ORIENTED_EDGE ( 'NONE', *, *, #7488, .T. ) ;
#7683 = DIRECTION ( 'NONE',  ( 0.000000000000000000, 0.000000000000000000, 1.000000000000000000 ) ) ;
#7684 = DIRECTION ( 'NONE',  ( 1.000000000000000000, 0.000000000000000000, 5.637851296924623057E-15 ) ) ;
#7685 = ORIENTED_EDGE ( 'NONE', *, *, #9134, .F. ) ;
#7686 = FACE_OUTER_BOUND ( 'NONE', #4796, .T. ) ;
#7687 = LINE ( 'NONE', #7034, #230 ) ;
#7688 = DIRECTION ( 'NONE',  ( -0.000000000000000000, -0.000000000000000000, -1.000000000000000000 ) ) ;
#7689 = CARTESIAN_POINT ( 'NONE',  ( -1.963858260114716980, 4.049832306626327316, 9.643948283277975264 ) ) ;
#7691 = ORIENTED_EDGE ( 'NONE', *, *, #9984, .T. ) ;
#7690 = VECTOR ( 'NONE', #9233, 1000.000000000000000 ) ;
#7692 = CARTESIAN_POINT ( 'NONE',  ( 0.000000000000000000, -10.00000000000000000, 0.000000000000000000 ) ) ;
#7693 = CARTESIAN_POINT ( 'NONE',  ( -2.000000000000013767, 15.00000000000000355, -3.999999999999988898 ) ) ;
#7694 = CARTESIAN_POINT ( 'NONE',  ( 0.000000000000000000, -0.7390083445627225744, -1.279999999999999138 ) ) ;
#7695 = PRODUCT_RELATED_PRODUCT_CATEGORY ( 'part', '', ( #9714 ) ) ;
#7696 = CIRCLE ( 'NONE', #6986, 3.000000000000000000 ) ;
#7697 = CARTESIAN_POINT ( 'NONE',  ( 0.000000000000000000, 0.000000000000000000, -12.00000000000000000 ) ) ;
#7698 = DIRECTION ( 'NONE',  ( 0.3420201433256627732, 0.9396926207859105373, 0.000000000000000000 ) ) ;
#7699 = CARTESIAN_POINT ( 'NONE',  ( 8.161409553233806236, -10.00000000000000000, -12.00000000000000000 ) ) ;
#7700 = CARTESIAN_POINT ( 'NONE',  ( 10.00000000000000000, 0.005878491403557128264, -7.047692205288322853 ) ) ;
#7701 = CARTESIAN_POINT ( 'NONE',  ( 3.181980515339458471, 3.181980515339470461, 2.232096619617652273E-17 ) ) ;
#7702 = DIRECTION ( 'NONE',  ( 1.000000000000000000, 0.000000000000000000, 0.000000000000000000 ) ) ;
#7703 = CARTESIAN_POINT ( 'NONE',  ( 2.231261971483764484, 4.173491630687871101, 10.06394828327797519 ) ) ;
#7704 = FACE_OUTER_BOUND ( 'NONE', #8094, .T. ) ;
#7705 = AXIS2_PLACEMENT_3D ( 'NONE', #3594, #4591, #3539 ) ;
#7706 = EDGE_LOOP ( 'NONE', ( #8559, #9090, #5699, #5915 ) ) ;
#7707 = DIRECTION ( 'NONE',  ( -1.000000000000000000, -0.000000000000000000, -0.000000000000000000 ) ) ;
#7708 = AXIS2_PLACEMENT_3D ( 'NONE', #1942, #5166, #8415 ) ;
#7709 = DIRECTION ( 'NONE',  ( 0.000000000000000000, 1.000000000000000000, 0.000000000000000000 ) ) ;
#7710 = DIRECTION ( 'NONE',  ( 1.000000000000000000, 0.000000000000000000, -0.000000000000000000 ) ) ;
#7711 = DIRECTION ( 'NONE',  ( 0.000000000000000000, 0.000000000000000000, 1.000000000000000000 ) ) ;
#7712 = ORIENTED_EDGE ( 'NONE', *, *, #9786, .F. ) ;
#7713 = CIRCLE ( 'NONE', #1110, 0.5000000000000000000 ) ;
#7714 = ADVANCED_FACE ( 'NONE', ( #5339 ), #8582, .T. ) ;
#7715 = CARTESIAN_POINT ( 'NONE',  ( -4.673326407553653361, 0.7401821875142517992, 13.01999999999999602 ) ) ;
#7716 = CARTESIAN_POINT ( 'NONE',  ( 0.7401821875142697849, -4.673326407553650697, 6.579999999999999183 ) ) ;
#7717 = CARTESIAN_POINT ( 'NONE',  ( -1.229367062500000163, -12.29022459553277002, -1.135416667349463227 ) ) ;
#7718 = ORIENTED_EDGE ( 'NONE', *, *, #5222, .F. ) ;
#7719 = VECTOR ( 'NONE', #10196, 1000.000000000000000 ) ;
#7720 = ORIENTED_EDGE ( 'NONE', *, *, #705, .F. ) ;
#7721 = CARTESIAN_POINT ( 'NONE',  ( 1.500000000000000222, -13.00000000000000533, -2.500000000000000000 ) ) ;
#7722 = AXIS2_PLACEMENT_3D ( 'NONE', #8452, #6043, #8557 ) ;
#7723 = DIRECTION ( 'NONE',  ( -1.000000000000000000, -0.000000000000000000, 0.000000000000000000 ) ) ;
#7724 = DIRECTION ( 'NONE',  ( 1.000000000000000000, 0.000000000000000000, 0.000000000000000000 ) ) ;
#7725 = EDGE_LOOP ( 'NONE', ( #2309, #8487, #45 ) ) ;
#7726 = EDGE_CURVE ( 'NONE', #5109, #2579, #570, .T. ) ;
#7727 = CARTESIAN_POINT ( 'NONE',  ( -2.576046737280769605, 4.860232935257343456, 8.836051716722023386 ) ) ;
#7728 = EDGE_CURVE ( 'NONE', #9979, #10188, #3065, .T. ) ;
#7729 = CARTESIAN_POINT ( 'NONE',  ( 2.496947748567516889, -4.900535883036019946, 9.240000000000000213 ) ) ;
#7730 = CARTESIAN_POINT ( 'NONE',  ( -0.8603895577212598011, -5.432285873273260179, 6.719999999999999751 ) ) ;
#7731 = EDGE_LOOP ( 'NONE', ( #1265, #9539, #9108, #7819 ) ) ;
#7732 = CARTESIAN_POINT ( 'NONE',  ( 0.7500000000000003331, -11.70096189432334732, -1.479166668032260157 ) ) ;
#7733 = ORIENTED_EDGE ( 'NONE', *, *, #9463, .F. ) ;
#7734 = CARTESIAN_POINT ( 'NONE',  ( 23.25451694676619496, -10.00000000000000000, -12.00000000000000000 ) ) ;
#7735 = CARTESIAN_POINT ( 'NONE',  ( 13.01080596966725622, -7.750000000000000000, -12.00000000000000000 ) ) ;
#7736 = ORIENTED_EDGE ( 'NONE', *, *, #3307, .F. ) ;
#7737 = EDGE_CURVE ( 'NONE', #2911, #2633, #3115, .T. ) ;
#7738 = DIRECTION ( 'NONE',  ( -1.000000000000000000, -0.000000000000000000, -0.000000000000000000 ) ) ;
#7739 = CARTESIAN_POINT ( 'NONE',  ( 1.272613240716556016, 6.025400000000000311, -12.00000000000000000 ) ) ;
#7740 = CARTESIAN_POINT ( 'NONE',  ( 2.231261971483764484, 4.173491630687871101, 10.06394828327797519 ) ) ;
#7741 = ORIENTED_EDGE ( 'NONE', *, *, #9955, .T. ) ;
#7742 = LINE ( 'NONE', #9386, #5591 ) ;
#7743 = EDGE_CURVE ( 'NONE', #1390, #9757, #5494, .T. ) ;
#7744 = FACE_OUTER_BOUND ( 'NONE', #8847, .T. ) ;
#7745 = DIRECTION ( 'NONE',  ( 1.000000000000000000, 0.000000000000000000, 0.000000000000000000 ) ) ;
#7746 = PRODUCT ( 'position sensor magnet', 'position sensor magnet', '', ( #8704 ) ) ;
#7747 = LINE ( 'NONE', #481, #9745 ) ;
#7748 = LINE ( 'NONE', #482, #8637 ) ;
#7749 = CARTESIAN_POINT ( 'NONE',  ( 8.000000000000001776, 7.008469740302810891, 2.257469275785291440 ) ) ;
#7750 = DIRECTION ( 'NONE',  ( 0.000000000000000000, 0.000000000000000000, -1.000000000000000000 ) ) ;
#7751 = CARTESIAN_POINT ( 'NONE',  ( -2.500000000000000000, 0.000000000000000000, 3.000000000000000000 ) ) ;
#7752 = CARTESIAN_POINT ( 'NONE',  ( -4.215868657802586128, -2.148092372876348133, 1.540000000000000036 ) ) ;
#7753 = CARTESIAN_POINT ( 'NONE',  ( 1.229367062500000385, -12.29022459553277002, -2.302083334016129967 ) ) ;
#7754 = CARTESIAN_POINT ( 'NONE',  ( 2.231261971483764484, 4.173491630687871101, 12.86394828327797768 ) ) ;
#7755 = CARTESIAN_POINT ( 'NONE',  ( 0.6146835312499993043, -14.06466310670085562, -0.8020833340161299674 ) ) ;
#7756 = ORIENTED_EDGE ( 'NONE', *, *, #2039, .F. ) ;
#7757 = LINE ( 'NONE', #6257, #3398 ) ;
#7758 = CARTESIAN_POINT ( 'NONE',  ( 3.889087296526005488, 3.889087296526018811, -3.866961113726609188E-17 ) ) ;
#7759 = CARTESIAN_POINT ( 'NONE',  ( 3.000000000000000888, 0.000000000000000000, 0.000000000000000000 ) ) ;
#7760 = DIRECTION ( 'NONE',  ( 0.000000000000000000, 1.000000000000000000, 0.000000000000000000 ) ) ;
#7761 = VERTEX_POINT ( 'NONE', #8057 ) ;
#7762 = CARTESIAN_POINT ( 'NONE',  ( -1.500000000000000222, -13.00000000000000533, -0.3125000013655936937 ) ) ;
#7763 = ADVANCED_FACE ( 'NONE', ( #7082 ), #8735, .F. ) ;
#7764 = CARTESIAN_POINT ( 'NONE',  ( 3.586028019667255595, 3.750000000000000000, 0.000000000000000000 ) ) ;
#7765 = CARTESIAN_POINT ( 'NONE',  ( 2.042957248827968808, -4.009529358847652603, 3.639999999999999680 ) ) ;
#7766 = CARTESIAN_POINT ( 'NONE',  ( 1.229367062500000385, -12.29022459553277002, -1.802083334016129967 ) ) ;
#7767 = ORIENTED_EDGE ( 'NONE', *, *, #2816, .F. ) ;
#7768 = EDGE_CURVE ( 'NONE', #346, #4853, #5913, .T. ) ;
#7769 = ORIENTED_EDGE ( 'NONE', *, *, #8869, .T. ) ;
#7770 = DIRECTION ( 'NONE',  ( -1.000000000000000000, -0.000000000000000000, -0.000000000000000000 ) ) ;
#7771 = DIRECTION ( 'NONE',  ( 0.000000000000000000, 0.000000000000000000, 1.000000000000000000 ) ) ;
#7772 = ORIENTED_EDGE ( 'NONE', *, *, #7853, .T. ) ;
#7773 = CARTESIAN_POINT ( 'NONE',  ( -5.726445515403654873, 0.8124729078101847746, 5.616051716722022746 ) ) ;
#7774 = AXIS2_PLACEMENT_3D ( 'NONE', #7700, #1227, #4452 ) ;
#7775 = SURFACE_STYLE_USAGE ( .BOTH. , #2157 ) ;
#7776 = ORIENTED_EDGE ( 'NONE', *, *, #5222, .T. ) ;
#7777 = STYLED_ITEM ( 'NONE', ( #3058 ), #4435 ) ;
#7778 = FACE_OUTER_BOUND ( 'NONE', #1935, .T. ) ;
#7779 = VERTEX_POINT ( 'NONE', #678 ) ;
#7780 = ORIENTED_EDGE ( 'NONE', *, *, #3812, .T. ) ;
#7781 = EDGE_CURVE ( 'NONE', #6751, #5863, #4808, .T. ) ;
#7782 = DIRECTION ( 'NONE',  ( 0.000000000000000000, -0.5150380749100571531, -0.8571673007021105573 ) ) ;
#7783 = AXIS2_PLACEMENT_3D ( 'NONE', #2578, #4057, #7294 ) ;
#7784 = DIRECTION ( 'NONE',  ( 0.000000000000000000, 0.000000000000000000, -1.000000000000000000 ) ) ;
#7785 = VERTEX_POINT ( 'NONE', #2221 ) ;
#7786 = DIRECTION ( 'NONE',  ( 0.000000000000000000, 0.000000000000000000, -1.000000000000000000 ) ) ;
#7787 = CARTESIAN_POINT ( 'NONE',  ( 0.000000000000000000, -10.00000000000000000, 0.000000000000000000 ) ) ;
#7788 = CARTESIAN_POINT ( 'NONE',  ( -4.860232935257354114, 2.576046737280751842, 3.763948283277976703 ) ) ;
#7789 = ORIENTED_EDGE ( 'NONE', *, *, #8101, .T. ) ;
#7790 = AXIS2_PLACEMENT_3D ( 'NONE', #420, #6875, #6923 ) ;
#7791 = CARTESIAN_POINT ( 'NONE',  ( 10.00000000000000000, -2.861184399890952079, -6.440778198864142823 ) ) ;
#7792 = AXIS2_PLACEMENT_3D ( 'NONE', #7992, #3005, #10223 ) ;
#7793 = CARTESIAN_POINT ( 'NONE',  ( 10.00000000000000000, 5.904264776415129923, -2.046865518294644914 ) ) ;
#7794 = ADVANCED_FACE ( 'NONE', ( #7246 ), #9706, .F. ) ;
#7795 = SURFACE_STYLE_FILL_AREA ( #4703 ) ;
#7796 = EDGE_CURVE ( 'NONE', #2259, #6255, #4695, .T. ) ;
#7797 = DIRECTION ( 'NONE',  ( -1.000000000000000000, 0.000000000000000000, 0.000000000000000000 ) ) ;
#7798 = CIRCLE ( 'NONE', #347, 6.248999999999999666 ) ;
#7799 = LINE ( 'NONE', #8694, #7283 ) ;
#7800 = CARTESIAN_POINT ( 'NONE',  ( -26.99999999999998934, -35.00000000000000000, 9.000000000000000000 ) ) ;
#7801 = VECTOR ( 'NONE', #2197, 1000.000000000000000 ) ;
#7802 = CARTESIAN_POINT ( 'NONE',  ( 0.000000000000000000, 6.000000000000000000, -12.00000000000000000 ) ) ;
#7803 = VECTOR ( 'NONE', #6930, 1000.000000000000000 ) ;
#7804 = LINE ( 'NONE', #538, #8114 ) ;
#7805 = CARTESIAN_POINT ( 'NONE',  ( -0.8323763977770610722, 4.658724279160015413, 14.57605171672202538 ) ) ;
#7806 = CARTESIAN_POINT ( 'NONE',  ( 0.6146835312500001924, -11.93533689329915326, -2.760416667349463449 ) ) ;
#7807 = CIRCLE ( 'NONE', #1881, 2.000000000000000000 ) ;
#7808 = AXIS2_PLACEMENT_3D ( 'NONE', #8354, #2778, #1185 ) ;
#7809 = CARTESIAN_POINT ( 'NONE',  ( -2.417848759854264618, 4.940838830814694660, 6.843948283277976330 ) ) ;
#7810 = ADVANCED_FACE ( 'NONE', ( #6287 ), #8001, .T. ) ;
#7811 = CARTESIAN_POINT ( 'NONE',  ( 0.6146835312500001924, -11.93533689329915326, -0.1354166673494631989 ) ) ;
#7813 = ORIENTED_EDGE ( 'NONE', *, *, #9146, .F. ) ;
#7812 = CIRCLE ( 'NONE', #2731, 2.600000000000000089 ) ;
#7814 = LINE ( 'NONE', #1444, #8143 ) ;
#7815 = CIRCLE ( 'NONE', #3410, 8.500000000000000000 ) ;
#7816 = CARTESIAN_POINT ( 'NONE',  ( 8.980342580332745683, 3.750000000000000000, 0.000000000000000000 ) ) ;
#7817 = LINE ( 'NONE', #709, #9245 ) ;
#7818 = CARTESIAN_POINT ( 'NONE',  ( -0.7500000000000007772, -14.29903810567666156, -1.666666666666666741 ) ) ;
#7819 = ORIENTED_EDGE ( 'NONE', *, *, #9365, .T. ) ;
#7820 = DIRECTION ( 'NONE',  ( 0.000000000000000000, 0.000000000000000000, -1.000000000000000000 ) ) ;
#7821 = CARTESIAN_POINT ( 'NONE',  ( 20.71853530928344611, 6.025400000000000311, -12.00000000000000000 ) ) ;
#7822 = CARTESIAN_POINT ( 'NONE',  ( -4.049832306626335310, 1.963858260114700327, 14.15605171672202012 ) ) ;
#7823 = CARTESIAN_POINT ( 'NONE',  ( 1.229367062499999719, -13.70977540446724063, -1.385416667349463671 ) ) ;
#7824 = VERTEX_POINT ( 'NONE', #3854 ) ;
#7825 = ORIENTED_EDGE ( 'NONE', *, *, #9453, .T. ) ;
#7826 = DIRECTION ( 'NONE',  ( -1.000000000000000000, 0.000000000000000000, 0.000000000000000000 ) ) ;
#7827 = DIRECTION ( 'NONE',  ( 1.000000000000000000, -0.000000000000000000, -0.000000000000000000 ) ) ;
#7828 = ORIENTED_EDGE ( 'NONE', *, *, #7664, .T. ) ;
#7829 = CARTESIAN_POINT ( 'NONE',  ( 5.418398423912711870, 0.9480714621563913758, 12.47605171672202218 ) ) ;
#7830 = DIRECTION ( 'NONE',  ( 0.000000000000000000, -0.000000000000000000, 1.000000000000000000 ) ) ;
#7831 = ORIENTED_EDGE ( 'NONE', *, *, #2671, .T. ) ;
#7832 = EDGE_LOOP ( 'NONE', ( #8990, #6180, #9269, #8830, #3113, #7310, #6280, #3601 ) ) ;
#7833 = EDGE_LOOP ( 'NONE', ( #9866, #824, #4274, #1186, #8521 ) ) ;
#7834 = LINE ( 'NONE', #9486, #8903 ) ;
#7835 = DIRECTION ( 'NONE',  ( 1.000000000000000000, 0.000000000000000000, -0.000000000000000000 ) ) ;
#7836 = ORIENTED_EDGE ( 'NONE', *, *, #9693, .F. ) ;
#7837 = DIRECTION ( 'NONE',  ( 0.000000000000000000, 0.000000000000000000, -1.000000000000000000 ) ) ;
#7838 = LINE ( 'NONE', #1267, #2597 ) ;
#7839 = CARTESIAN_POINT ( 'NONE',  ( 4.023224611898322145, -4.155232146225737111, 5.303948283277975406 ) ) ;
#7840 = VERTEX_POINT ( 'NONE', #2270 ) ;
#7841 = EDGE_CURVE ( 'NONE', #9951, #4800, #5652, .T. ) ;
#7842 = VECTOR ( 'NONE', #2186, 1000.000000000000000 ) ;
#7843 = DIRECTION ( 'NONE',  ( 0.000000000000000000, 0.000000000000000000, -1.000000000000000000 ) ) ;
#7844 = FACE_OUTER_BOUND ( 'NONE', #8529, .T. ) ;
#7845 = CARTESIAN_POINT ( 'NONE',  ( 1.499999999999999778, -13.86602540378444637, -0.04166666666666685170 ) ) ;
#7846 = CARTESIAN_POINT ( 'NONE',  ( 5.010572059283444624, 6.025400000000000311, -12.00000000000000000 ) ) ;
#7847 = CIRCLE ( 'NONE', #6486, 1.500000000000000222 ) ;
#7848 = DIRECTION ( 'NONE',  ( 1.000000000000000000, 0.000000000000000000, -0.000000000000000000 ) ) ;
#7849 = CARTESIAN_POINT ( 'NONE',  ( 8.000000000000001776, 5.904264776415129923, -2.046865518294644914 ) ) ;
#7850 = DIRECTION ( 'NONE',  ( 0.000000000000000000, 0.000000000000000000, 1.000000000000000000 ) ) ;
#7851 = CARTESIAN_POINT ( 'NONE',  ( 3.181980515339458471, 3.181980515339470461, 5.599999999999998757 ) ) ;
#7852 = EDGE_CURVE ( 'NONE', #9335, #9691, #6937, .T. ) ;
#7853 = EDGE_CURVE ( 'NONE', #5636, #8002, #1875, .T. ) ;
#7854 = CARTESIAN_POINT ( 'NONE',  ( -1.229367062500000163, -12.29022459553277002, -2.635416667349463449 ) ) ;
#7855 = CARTESIAN_POINT ( 'NONE',  ( -5.446173322633801384, -0.7727076532861678615, 9.083948283277974767 ) ) ;
#7856 = STYLED_ITEM ( 'NONE', ( #3920 ), #8040 ) ;
#7857 = CARTESIAN_POINT ( 'NONE',  ( 0.000000000000000000, 6.000000000000000000, -12.00000000000000000 ) ) ;
#7858 = EDGE_LOOP ( 'NONE', ( #2648, #9072, #1467, #5430, #5345, #2166, #7106, #5189, #4631, #6294, #1634, #3207, #5242, #2956, #5650, #5019, #197, #7666, #10012, #8794, #6069, #7610, #9601, #3985, #7134, #9697, #7733, #7241, #4626, #1308, #8163, #2262, #8177, #2805, #5939, #7925 ) ) ;
#7859 =( NAMED_UNIT ( * ) SI_UNIT ( $, .STERADIAN. ) SOLID_ANGLE_UNIT ( ) );
#7860 = CARTESIAN_POINT ( 'NONE',  ( -1.500000000000000222, -13.00000000000000533, -2.312500001365593860 ) ) ;
#7861 = CARTESIAN_POINT ( 'NONE',  ( 12.75489823682933554, 10.64240329930025375, 0.000000000000000000 ) ) ;
#7862 = DIRECTION ( 'NONE',  ( 0.000000000000000000, 0.000000000000000000, 1.000000000000000000 ) ) ;
#7863 = MECHANICAL_DESIGN_GEOMETRIC_PRESENTATION_REPRESENTATION (  '', ( #2114 ), #4818 ) ;
#7864 = DIRECTION ( 'NONE',  ( 0.000000000000000000, 0.000000000000000000, 1.000000000000000000 ) ) ;
#7865 = ORIENTED_EDGE ( 'NONE', *, *, #7852, .F. ) ;
#7866 = EDGE_CURVE ( 'NONE', #8200, #6255, #1836, .T. ) ;
#7867 = CARTESIAN_POINT ( 'NONE',  ( -3.181725716174720991E-16, -14.73205080756888563, -0.1875000013655935827 ) ) ;
#7868 = CARTESIAN_POINT ( 'NONE',  ( 23.86937280323380506, -10.00000000000000000, -12.00000000000000000 ) ) ;
#7869 = VECTOR ( 'NONE', #3193, 1000.000000000000000 ) ;
#7870 = CARTESIAN_POINT ( 'NONE',  ( -4.444597532678119300, -0.7039550926810477227, 7.279999999999999361 ) ) ;
#7871 = LINE ( 'NONE', #239, #9199 ) ;
#7872 = PRODUCT_DEFINITION_FORMATION_WITH_SPECIFIED_SOURCE ( 'ANY', '', #7331, .NOT_KNOWN. ) ;
#7873 = ORIENTED_EDGE ( 'NONE', *, *, #8272, .F. ) ;
#7874 = VERTEX_POINT ( 'NONE', #836 ) ;
#7875 = CARTESIAN_POINT ( 'NONE',  ( 0.7500000000000003331, -11.70096189432334732, -0.9166666666666667407 ) ) ;
#7876 = AXIS2_PLACEMENT_3D ( 'NONE', #1445, #5467, #356 ) ;
#7877 = FILL_AREA_STYLE ('',( #9531 ) ) ;
#7878 = VERTEX_POINT ( 'NONE', #4068 ) ;
#7879 = CARTESIAN_POINT ( 'NONE',  ( -2.542276634908081423, -5.195105386651227342, 13.45605171672202260 ) ) ;
#7880 = CARTESIAN_POINT ( 'NONE',  ( 3.586028019667255595, -7.750000000000000000, 0.000000000000000000 ) ) ;
#7881 = CARTESIAN_POINT ( 'NONE',  ( -2.000000000000000000, 7.008469740302802897, 0.7425307242148025955 ) ) ;
#7882 = VERTEX_POINT ( 'NONE', #8682 ) ;
#7883 = CARTESIAN_POINT ( 'NONE',  ( -1.499999999999998224, -12.13397459621556607, -1.354166668032260379 ) ) ;
#7884 = CARTESIAN_POINT ( 'NONE',  ( -4.155232146225753098, 4.023224611898306158, 11.49605171672201998 ) ) ;
#7885 = CIRCLE ( 'NONE', #3998, 1.249999999999988898 ) ;
#7886 = VERTEX_POINT ( 'NONE', #7304 ) ;
#7887 = VECTOR ( 'NONE', #6527, 1000.000000000000000 ) ;
#7888 = ORIENTED_EDGE ( 'NONE', *, *, #7532, .F. ) ;
#7889 = DIRECTION ( 'NONE',  ( 0.000000000000000000, 0.000000000000000000, -1.000000000000000000 ) ) ;
#7890 = DIRECTION ( 'NONE',  ( 0.000000000000000000, -1.000000000000000000, -0.000000000000000000 ) ) ;
#7891 = ORIENTED_EDGE ( 'NONE', *, *, #10343, .T. ) ;
#7892 = DIRECTION ( 'NONE',  ( 0.000000000000000000, 0.000000000000000000, 1.000000000000000000 ) ) ;
#7893 = VECTOR ( 'NONE', #9717, 1000.000000000000000 ) ;
#7894 = CARTESIAN_POINT ( 'NONE',  ( -2.000000000000000000, 0.000000000000000000, 0.000000000000000000 ) ) ;
#7895 = CARTESIAN_POINT ( 'NONE',  ( -2.417848759854264618, 4.940838830814694660, 6.843948283277976330 ) ) ;
#7896 = ORIENTED_EDGE ( 'NONE', *, *, #5956, .F. ) ;
#7897 = AXIS2_PLACEMENT_3D ( 'NONE', #7802, #3080, #5352 ) ;
#7898 = CARTESIAN_POINT ( 'NONE',  ( 4.000000000000000888, 0.6700234925293845345, -8.473551116235670477 ) ) ;
#7899 = EDGE_CURVE ( 'NONE', #292, #3947, #1418, .T. ) ;
#7900 = CYLINDRICAL_SURFACE ( 'NONE', #2941, 6.248999999999999666 ) ;
#7901 = DIRECTION ( 'NONE',  ( -1.000000000000000000, 0.000000000000000000, 0.000000000000000000 ) ) ;
#7902 = DIRECTION ( 'NONE',  ( 0.000000000000000000, 0.000000000000000000, 1.000000000000000000 ) ) ;
#7903 = ADVANCED_FACE ( 'NONE', ( #8211 ), #1897, .F. ) ;
#7904 = CARTESIAN_POINT ( 'NONE',  ( -1.499999999999996891, -12.13397459621556429, -2.291666666666666519 ) ) ;
#7905 = CARTESIAN_POINT ( 'NONE',  ( 3.586028019667255595, 3.750000000000000000, -12.00000000000000000 ) ) ;
#7906 = DIRECTION ( 'NONE',  ( 0.000000000000000000, 0.000000000000000000, 1.000000000000000000 ) ) ;
#7907 = CARTESIAN_POINT ( 'NONE',  ( 0.7401821875142697849, -4.673326407553650697, 3.779999999999998472 ) ) ;
#7908 = CARTESIAN_POINT ( 'NONE',  ( -1.229367062500000163, -12.29022459553277002, -2.135416667349463449 ) ) ;
#7909 = CARTESIAN_POINT ( 'NONE',  ( -5.697241258616385196, 0.9968613283357647958, 9.223948283277977112 ) ) ;
#7910 = FACE_OUTER_BOUND ( 'NONE', #4160, .T. ) ;
#7911 = ORIENTED_EDGE ( 'NONE', *, *, #7737, .T. ) ;
#7912 = APPLICATION_PROTOCOL_DEFINITION ( 'draft international standard', 'automotive_design', 1998, #10355 ) ;
#7913 = ADVANCED_FACE ( 'NONE', ( #306, #8944 ), #8317, .F. ) ;
#7914 = DIRECTION ( 'NONE',  ( 0.3420201433256627732, -0.9396926207859105373, 0.000000000000000000 ) ) ;
#7915 = EDGE_CURVE ( 'NONE', #2738, #9761, #4171, .T. ) ;
#7916 = DIRECTION ( 'NONE',  ( 0.000000000000000000, 1.000000000000000000, 0.000000000000000000 ) ) ;
#7917 = LINE ( 'NONE', #3878, #7640 ) ;
#7918 = LINE ( 'NONE', #6472, #7887 ) ;
#7919 = FACE_OUTER_BOUND ( 'NONE', #658, .T. ) ;
#7920 = EDGE_LOOP ( 'NONE', ( #7184, #5119, #8733, #2874 ) ) ;
#7921 = CARTESIAN_POINT ( 'NONE',  ( 10.69739119071655686, 6.025400000000000311, -12.00000000000000000 ) ) ;
#7922 = CARTESIAN_POINT ( 'NONE',  ( -3.181980515339458027, -3.181980515339470905, 6.999999999999999112 ) ) ;
#7923 = UNCERTAINTY_MEASURE_WITH_UNIT (LENGTH_MEASURE( 1.000000000000000082E-05 ), #6763, 'distance_accuracy_value', 'NONE');
#7924 = CARTESIAN_POINT ( 'NONE',  ( 1.500000000000000444, -12.13397459621556607, -0.4583333333333336479 ) ) ;
#7925 = ORIENTED_EDGE ( 'NONE', *, *, #3902, .F. ) ;
#7926 = ADVANCED_FACE ( 'NONE', ( #7563 ), #5752, .T. ) ;
#7927 = ORIENTED_EDGE ( 'NONE', *, *, #6326, .T. ) ;
#7928 = DIRECTION ( 'NONE',  ( 1.000000000000000000, 0.000000000000000000, 0.000000000000000000 ) ) ;
#7929 = CARTESIAN_POINT ( 'NONE',  ( 3.586028019667255595, 3.750000000000000000, -12.00000000000000000 ) ) ;
#7930 = ORIENTED_EDGE ( 'NONE', *, *, #5583, .F. ) ;
#7931 = CARTESIAN_POINT ( 'NONE',  ( -3.826313983664925811, -3.951860609387098489, 10.79605171672202246 ) ) ;
#7932 = FACE_OUTER_BOUND ( 'NONE', #9426, .T. ) ;
#7933 = ORIENTED_EDGE ( 'NONE', *, *, #7107, .T. ) ;
#7934 = CARTESIAN_POINT ( 'NONE',  ( 0.000000000000000000, 3.750000000000000000, -12.00000000000000000 ) ) ;
#7935 = CARTESIAN_POINT ( 'NONE',  ( 3.826313983664925811, 3.951860609387098044, 12.19605171672202282 ) ) ;
#7936 = EDGE_LOOP ( 'NONE', ( #4112, #2038, #3230, #1162 ) ) ;
#7937 = EDGE_CURVE ( 'NONE', #3241, #10315, #3529, .T. ) ;
#7938 = ORIENTED_EDGE ( 'NONE', *, *, #5582, .T. ) ;
#7939 = CARTESIAN_POINT ( 'NONE',  ( 13.01080596966725622, 3.750000000000000000, 0.000000000000000000 ) ) ;
#7940 = VECTOR ( 'NONE', #7688, 1000.000000000000000 ) ;
#7941 = DIRECTION ( 'NONE',  ( -1.000000000000000000, -0.000000000000000000, -0.000000000000000000 ) ) ;
#7942 = VERTEX_POINT ( 'NONE', #1687 ) ;
#7943 = DIRECTION ( 'NONE',  ( 0.000000000000000000, 0.000000000000000000, 1.000000000000000000 ) ) ;
#7944 = CARTESIAN_POINT ( 'NONE',  ( 0.000000000000000000, -4.000000000000000000, 0.000000000000000000 ) ) ;
#7945 = CARTESIAN_POINT ( 'NONE',  ( -3.951860609387083834, -3.826313983664940466, 3.203948283277977094 ) ) ;
#7946 = VERTEX_POINT ( 'NONE', #4914 ) ;
#7947 = CARTESIAN_POINT ( 'NONE',  ( 0.7500000000000003331, -11.70096189432334732, -0.9791666680322602678 ) ) ;
#7948 = VECTOR ( 'NONE', #8561, 1000.000000000000000 ) ;
#7949 = CARTESIAN_POINT ( 'NONE',  ( 1.060575238724907038E-16, -11.26794919243112680, -0.4375000013655938602 ) ) ;
#7950 = FACE_BOUND ( 'NONE', #2901, .T. ) ;
#7951 = AXIS2_PLACEMENT_3D ( 'NONE', #3015, #2117, #7943 ) ;
#7952 = MANIFOLD_SOLID_BREP ( 'Extrude-Thin1', #431 ) ;
#7953 = EDGE_LOOP ( 'NONE', ( #9765, #2837, #10489, #9165 ) ) ;
#7954 = SHAPE_REPRESENTATION ( 'cover', ( #2101 ), #4472 ) ;
#7955 = CARTESIAN_POINT ( 'NONE',  ( 1.300000000000000044, 1.567547902908612085E-16, -1.280000000000000027 ) ) ;
#7956 = CLOSED_SHELL ( 'NONE', ( #5732, #9997, #107, #7437, #5046, #797, #7994, #5553, #2641, #148, #7585, #3405, #7340, #3188, #3964, #6872, #7714, #10039, #2351, #161, #9083, #9749, #1341, #1765 ) ) ;
#7957 = DIRECTION ( 'NONE',  ( 0.000000000000000000, 0.000000000000000000, 1.000000000000000000 ) ) ;
#7958 = LINE ( 'NONE', #6460, #3886 ) ;
#7959 = PLANE ( 'NONE',  #9252 ) ;
#7960 = VECTOR ( 'NONE', #3168, 1000.000000000000000 ) ;
#7961 = DIRECTION ( 'NONE',  ( 0.000000000000000000, -1.000000000000000000, -0.000000000000000000 ) ) ;
#7962 = CARTESIAN_POINT ( 'NONE',  ( -4.673326407553653361, 0.7401821875142517992, 7.419999999999998153 ) ) ;
#7963 = CARTESIAN_POINT ( 'NONE',  ( 0.6146835312500001924, -11.93533689329915326, -1.260416667349463227 ) ) ;
#7964 = EDGE_CURVE ( 'NONE', #8145, #48, #9805, .T. ) ;
#7965 = CARTESIAN_POINT ( 'NONE',  ( 5.446173322633801384, 0.7727076532861675284, 7.683948283277975300 ) ) ;
#7966 = LINE ( 'NONE', #8022, #5961 ) ;
#7967 = COLOUR_RGB ( '', 0.66274510, 0.83137255, 0.94901961) ;
#7968 = ORIENTED_EDGE ( 'NONE', *, *, #10325, .F. ) ;
#7969 = SHAPE_DEFINITION_REPRESENTATION ( #9446, #7207 ) ;
#7970 = CIRCLE ( 'NONE', #5411, 8.500000000000000000 ) ;
#7971 = DIRECTION ( 'NONE',  ( 0.000000000000000000, 0.000000000000000000, -1.000000000000000000 ) ) ;
#7972 = CARTESIAN_POINT ( 'NONE',  ( -3.181725716174720991E-16, -14.73205080756888563, -1.687500001365593638 ) ) ;
#7973 = EDGE_LOOP ( 'NONE', ( #9707, #7873, #1045, #4575 ) ) ;
#7974 = CARTESIAN_POINT ( 'NONE',  ( 30.00000000000001066, 35.00000000000001421, 9.000000000000000000 ) ) ;
#7975 = CARTESIAN_POINT ( 'NONE',  ( 8.000000000000001776, -7.063614741696270016, 3.730353617970412206 ) ) ;
#7976 = VECTOR ( 'NONE', #8505, 1000.000000000000000 ) ;
#7977 = DIRECTION ( 'NONE',  ( 1.000000000000000000, 0.000000000000000000, 0.000000000000000000 ) ) ;
#7978 = AXIS2_PLACEMENT_3D ( 'NONE', #3419, #4109, #4205 ) ;
#7979 = FACE_OUTER_BOUND ( 'NONE', #3420, .T. ) ;
#7980 = DIRECTION ( 'NONE',  ( 0.000000000000000000, 0.000000000000000000, 1.000000000000000000 ) ) ;
#7981 = EDGE_CURVE ( 'NONE', #2223, #7636, #2919, .T. ) ;
#7982 = CARTESIAN_POINT ( 'NONE',  ( -3.181980515339458027, -3.181980515339470905, 9.799999999999998934 ) ) ;
#7983 =( REPRESENTATION_RELATIONSHIP ('NONE','NONE', #5100, #13 ) REPRESENTATION_RELATIONSHIP_WITH_TRANSFORMATION ( #3347 )SHAPE_REPRESENTATION_RELATIONSHIP( ) );
#7984 = CARTESIAN_POINT ( 'NONE',  ( 0.7500000000000003331, -11.70096189432334732, -0.4166666666666667407 ) ) ;
#7985 = VERTEX_POINT ( 'NONE', #9055 ) ;
#7986 = VECTOR ( 'NONE', #882, 1000.000000000000000 ) ;
#7987 = ORIENTED_EDGE ( 'NONE', *, *, #8671, .T. ) ;
#7988 = CARTESIAN_POINT ( 'NONE',  ( -1.499999999999999778, -12.13397459621556784, -0.7916666666666666297 ) ) ;
#7989 = LINE ( 'NONE', #4900, #4752 ) ;
#7990 = EDGE_LOOP ( 'NONE', ( #6174, #2216, #1092 ) ) ;
#7991 = CARTESIAN_POINT ( 'NONE',  ( 0.6146835312499993043, -14.06466310670085562, 0.07291666598386974119 ) ) ;
#7992 = CARTESIAN_POINT ( 'NONE',  ( 11.00000000000000355, 0.000000000000000000, 0.000000000000000000 ) ) ;
#7993 = EDGE_LOOP ( 'NONE', ( #884, #8307 ) ) ;
#7994 = ADVANCED_FACE ( 'NONE', ( #3482 ), #206, .T. ) ;
#7995 = EDGE_CURVE ( 'NONE', #1802, #10462, #9107, .T. ) ;
#7996 = CARTESIAN_POINT ( 'NONE',  ( 8.000000000000001776, -0.1221666339523208161, -6.247805719894685694 ) ) ;
#7997 = CARTESIAN_POINT ( 'NONE',  ( -2.064922774268895811, -4.258245684917318918, 2.256051716722022871 ) ) ;
#7998 = ORIENTED_EDGE ( 'NONE', *, *, #1022, .T. ) ;
#7999 = VERTEX_POINT ( 'NONE', #2686 ) ;
#8000 = DIRECTION ( 'NONE',  ( 0.000000000000000000, 0.000000000000000000, 1.000000000000000000 ) ) ;
#8001 = CYLINDRICAL_SURFACE ( 'NONE', #4228, 3.000000000000000000 ) ;
#8002 = VERTEX_POINT ( 'NONE', #5904 ) ;
#8003 = CARTESIAN_POINT ( 'NONE',  ( 4.900535883036028828, -2.496947748567499126, 6.159999999999999254 ) ) ;
#8004 = CARTESIAN_POINT ( 'NONE',  ( 16.97133164676619899, 6.000000000000000000, -12.00000000000000000 ) ) ;
#8005 = CARTESIAN_POINT ( 'NONE',  ( -5.697241258616385196, 0.9968613283357647958, 0.8239482832779764232 ) ) ;
#8006 = VERTEX_POINT ( 'NONE', #2895 ) ;
#8007 = EDGE_CURVE ( 'NONE', #10490, #4313, #6911, .T. ) ;
#8008 = CARTESIAN_POINT ( 'NONE',  ( 1.500000000000000444, -12.13397459621556607, -0.02083333469892703974 ) ) ;
#8009 = DIRECTION ( 'NONE',  ( 0.000000000000000000, 0.000000000000000000, 1.000000000000000000 ) ) ;
#8010 = DIRECTION ( 'NONE',  ( -0.000000000000000000, 1.000000000000000000, -0.000000000000000000 ) ) ;
#8011 = VERTEX_POINT ( 'NONE', #5279 ) ;
#8012 = FACE_OUTER_BOUND ( 'NONE', #2539, .T. ) ;
#8013 = DIRECTION ( 'NONE',  ( 1.000000000000000000, 0.000000000000000000, 0.000000000000000000 ) ) ;
#8014 = DIRECTION ( 'NONE',  ( 0.000000000000000000, 0.000000000000000000, 1.000000000000000000 ) ) ;
#8015 = CARTESIAN_POINT ( 'NONE',  ( 2.500000000000007105, -28.99999999999999289, 0.000000000000000000 ) ) ;
#8016 = CIRCLE ( 'NONE', #3944, 2.000000000000003553 ) ;
#8017 = DIRECTION ( 'NONE',  ( -0.5000000000000034417, 0.000000000000000000, 0.8660254037844367092 ) ) ;
#8018 = CARTESIAN_POINT ( 'NONE',  ( 4.673326407553653361, -0.7401821875142523544, 3.219999999999999751 ) ) ;
#8019 = ORIENTED_EDGE ( 'NONE', *, *, #8874, .T. ) ;
#8020 = CARTESIAN_POINT ( 'NONE',  ( -2.607672531582950546E-16, -14.41955080893447416, -0.4687500006827967081 ) ) ;
#8021 = CARTESIAN_POINT ( 'NONE',  ( 5.697241258616385196, -0.9968613283357656840, 5.023948283277976046 ) ) ;
#8022 = CARTESIAN_POINT ( 'NONE',  ( 1.300000000000000044, -0.7390083445627200209, 1.280000000000001137 ) ) ;
#8023 = ORIENTED_EDGE ( 'NONE', *, *, #10380, .F. ) ;
#8024 = AXIS2_PLACEMENT_3D ( 'NONE', #4262, #8413, #1891 ) ;
#8025 = SHAPE_DEFINITION_REPRESENTATION ( #6474, #13 ) ;
#8026 = DIRECTION ( 'NONE',  ( 0.000000000000000000, 0.000000000000000000, 1.000000000000000000 ) ) ;
#8027 = LINE ( 'NONE', #8183, #4839 ) ;
#8028 = ORIENTED_EDGE ( 'NONE', *, *, #7438, .F. ) ;
#8029 = CARTESIAN_POINT ( 'NONE',  ( -2.000000000000024425, 15.00000000000000355, -5.999999999999988454 ) ) ;
#8030 = DIRECTION ( 'NONE',  ( 0.000000000000000000, 0.000000000000000000, 1.000000000000000000 ) ) ;
#8031 = EDGE_CURVE ( 'NONE', #10270, #8600, #4425, .T. ) ;
#8032 = DIRECTION ( 'NONE',  ( 0.3420201433256627732, 0.9396926207859105373, -0.000000000000000000 ) ) ;
#8033 = LINE ( 'NONE', #10483, #8963 ) ;
#8034 = CARTESIAN_POINT ( 'NONE',  ( 6.727620669667255804, 3.750000000000000000, -12.00000000000000000 ) ) ;
#8035 = PRESENTATION_LAYER_ASSIGNMENT (  '', '', ( #7856 ) ) ;
#8036 = CARTESIAN_POINT ( 'NONE',  ( 3.279728542977952799, -3.411736077305369541, -0.2960517167220233503 ) ) ;
#8037 = UNCERTAINTY_MEASURE_WITH_UNIT (LENGTH_MEASURE( 1.000000000000000082E-05 ), #5811, 'distance_accuracy_value', 'NONE');
#8038 = CARTESIAN_POINT ( 'NONE',  ( 0.7500000000000003331, -11.70096189432334732, -1.416666666666666741 ) ) ;
#8039 = ORIENTED_EDGE ( 'NONE', *, *, #9694, .T. ) ;
#8040 = ADVANCED_BREP_SHAPE_REPRESENTATION ( '', ( #4435, #2101 ), #4457 ) ;
#8041 = ORIENTED_EDGE ( 'NONE', *, *, #8700, .T. ) ;
#8042 = CIRCLE ( 'NONE', #1585, 6.248999999999999666 ) ;
#8043 = DIRECTION ( 'NONE',  ( 0.000000000000000000, 0.000000000000000000, -1.000000000000000000 ) ) ;
#8044 = EDGE_CURVE ( 'NONE', #3477, #7306, #3633, .T. ) ;
#8045 = ORIENTED_EDGE ( 'NONE', *, *, #7509, .T. ) ;
#8046 = CARTESIAN_POINT ( 'NONE',  ( 23.26376179071655770, 6.025400000000000311, -12.00000000000000000 ) ) ;
#8047 = CARTESIAN_POINT ( 'NONE',  ( 0.4444353696672553311, -7.750000000000000000, -12.00000000000000000 ) ) ;
#8048 = ORIENTED_EDGE ( 'NONE', *, *, #8095, .T. ) ;
#8049 = CARTESIAN_POINT ( 'NONE',  ( 0.6162731882459174804, 4.458484982038668498, 3.516051716722023102 ) ) ;
#8050 = ORIENTED_EDGE ( 'NONE', *, *, #8613, .F. ) ;
#8051 = SURFACE_SIDE_STYLE ('',( #5799 ) ) ;
#8052 = VECTOR ( 'NONE', #9660, 999.9999999999998863 ) ;
#8053 = ORIENTED_EDGE ( 'NONE', *, *, #9868, .F. ) ;
#8054 = EDGE_CURVE ( 'NONE', #8002, #5636, #8635, .T. ) ;
#8055 = DIRECTION ( 'NONE',  ( -1.000000000000000000, 0.000000000000000000, -0.000000000000000000 ) ) ;
#8056 = EDGE_CURVE ( 'NONE', #4568, #9536, #1300, .T. ) ;
#8057 = CARTESIAN_POINT ( 'NONE',  ( 10.00000000000000000, 7.008469740302810891, 2.257469275785291440 ) ) ;
#8058 = ORIENTED_EDGE ( 'NONE', *, *, #6377, .T. ) ;
#8059 = CARTESIAN_POINT ( 'NONE',  ( 5.711843387010018702, -0.9046671180729751738, 8.820000000000000284 ) ) ;
#8060 = DIRECTION ( 'NONE',  ( 0.000000000000000000, 0.000000000000000000, -1.000000000000000000 ) ) ;
#8061 = CARTESIAN_POINT ( 'NONE',  ( -4.900535883036028828, 2.496947748567499126, 4.759999999999999787 ) ) ;
#8062 = ORIENTED_EDGE ( 'NONE', *, *, #5631, .F. ) ;
#8063 = CARTESIAN_POINT ( 'NONE',  ( 1.500000000000000222, -13.00000000000000533, 0.4374999986344065284 ) ) ;
#8064 = AXIS2_PLACEMENT_3D ( 'NONE', #1562, #2409, #7862 ) ;
#8065 = VERTEX_POINT ( 'NONE', #6169 ) ;
#8066 = EDGE_CURVE ( 'NONE', #10267, #6226, #9368, .T. ) ;
#8067 = LINE ( 'NONE', #7955, #8052 ) ;
#8068 = VECTOR ( 'NONE', #455, 1000.000000000000000 ) ;
#8069 = CARTESIAN_POINT ( 'NONE',  ( -15.00000000000000000, 19.99999999999999645, 6.000000000000000000 ) ) ;
#8070 = CARTESIAN_POINT ( 'NONE',  ( -3.181725716174720991E-16, -14.73205080756888563, -2.125000000000000000 ) ) ;
#8071 = LINE ( 'NONE', #4438, #2696 ) ;
#8072 = CARTESIAN_POINT ( 'NONE',  ( 50.00005079999999680, 2.449293598294706414E-16, -2.000000000000000000 ) ) ;
#8073 = CARTESIAN_POINT ( 'NONE',  ( 4.009529358847659708, -2.042957248827953709, 6.159999999999999254 ) ) ;
#8074 = VERTEX_POINT ( 'NONE', #6116 ) ;
#8075 = CARTESIAN_POINT ( 'NONE',  ( 23.86937280323380506, 6.000000000000001776, 0.000000000000000000 ) ) ;
#8076 = CARTESIAN_POINT ( 'NONE',  ( -5.152728359536494551, -2.625446233515535077, 7.139999999999997016 ) ) ;
#8077 = DIRECTION ( 'NONE',  ( 0.000000000000000000, 0.000000000000000000, 1.000000000000000000 ) ) ;
#8078 = PRODUCT_CONTEXT ( 'NONE', #6884, 'mechanical' ) ;
#8079 = EDGE_CURVE ( 'NONE', #6457, #4313, #6056, .T. ) ;
#8080 = FACE_OUTER_BOUND ( 'NONE', #6907, .T. ) ;
#8081 = LINE ( 'NONE', #4143, #6002 ) ;
#8082 = LINE ( 'NONE', #812, #7213 ) ;
#8083 = CARTESIAN_POINT ( 'NONE',  ( 23.86012795928344588, 6.025400000000000311, -12.00000000000000000 ) ) ;
#8084 = FACE_OUTER_BOUND ( 'NONE', #5280, .T. ) ;
#8085 = CARTESIAN_POINT ( 'NONE',  ( -26.99999999999998934, -13.00000000000000533, 1.249999999999993339 ) ) ;
#8086 = CARTESIAN_POINT ( 'NONE',  ( 4.673326407553653361, -0.7401821875142523544, 11.61999999999999922 ) ) ;
#8087 = CARTESIAN_POINT ( 'NONE',  ( 1.500000000000000444, -12.13397459621556607, -2.458333333333333037 ) ) ;
#8088 = ADVANCED_FACE ( 'NONE', ( #10166 ), #5170, .T. ) ;
#8089 = ORIENTED_EDGE ( 'NONE', *, *, #6029, .T. ) ;
#8090 = EDGE_LOOP ( 'NONE', ( #9216, #508, #6850, #5478 ) ) ;
#8091 = LINE ( 'NONE', #6588, #1554 ) ;
#8092 = LINE ( 'NONE', #10381, #2391 ) ;
#8093 = EDGE_CURVE ( 'NONE', #8610, #7946, #853, .T. ) ;
#8094 = EDGE_LOOP ( 'NONE', ( #3220, #7831, #1684, #2553 ) ) ;
#8095 = EDGE_CURVE ( 'NONE', #4888, #2377, #2103, .T. ) ;
#8096 = CARTESIAN_POINT ( 'NONE',  ( 2.148092372876330369, 4.215868657802594122, 2.659999999999999254 ) ) ;
#8097 = CARTESIAN_POINT ( 'NONE',  ( -2.000000000000000000, -1.179494851233864106, -6.136676046192498291 ) ) ;
#8098 = EDGE_LOOP ( 'NONE', ( #5798, #269, #3173, #5275 ) ) ;
#8099 = CARTESIAN_POINT ( 'NONE',  ( 3.826313983664925811, 3.951860609387098044, 9.396051716722022107 ) ) ;
#8100 = PRODUCT_DEFINITION_SHAPE ( 'NONE', 'NONE',  #10501 ) ;
#8101 = EDGE_CURVE ( 'NONE', #2891, #2034, #3737, .T. ) ;
#8102 = ORIENTED_EDGE ( 'NONE', *, *, #4140, .F. ) ;
#8103 = ORIENTED_EDGE ( 'NONE', *, *, #5072, .F. ) ;
#8104 = CARTESIAN_POINT ( 'NONE',  ( 0.000000000000000000, -10.00000000000000000, -12.00000000000000000 ) ) ;
#8105 = CARTESIAN_POINT ( 'NONE',  ( -0.7499999999999997780, -11.70096189432334555, -1.833333333333333481 ) ) ;
#8106 = EDGE_LOOP ( 'NONE', ( #6765, #1132 ) ) ;
#8107 = CARTESIAN_POINT ( 'NONE',  ( -4.900535883036028828, 2.496947748567499126, 7.559999999999998721 ) ) ;
#8108 = PLANE ( 'NONE',  #5793 ) ;
#8109 = CARTESIAN_POINT ( 'NONE',  ( 0.9046671180729951578, -5.711843387010016926, 0.9799999999999997602 ) ) ;
#8110 = ORIENTED_EDGE ( 'NONE', *, *, #36, .T. ) ;
#8111 = CARTESIAN_POINT ( 'NONE',  ( 0.7499999999999991118, -14.29903810567666333, -0.6458333346989268975 ) ) ;
#8112 = EDGE_CURVE ( 'NONE', #165, #7946, #510, .T. ) ;
#8113 =( LENGTH_UNIT ( ) NAMED_UNIT ( * ) SI_UNIT ( .MILLI., .METRE. ) );
#8114 = VECTOR ( 'NONE', #6994, 1000.000000000000000 ) ;
#8115 = ORIENTED_EDGE ( 'NONE', *, *, #4588, .F. ) ;
#8116 = DIRECTION ( 'NONE',  ( -0.000000000000000000, -0.000000000000000000, -1.000000000000000000 ) ) ;
#8117 = DIRECTION ( 'NONE',  ( 1.000000000000000000, -0.000000000000000000, 0.000000000000000000 ) ) ;
#8118 = DIRECTION ( 'NONE',  ( 0.000000000000000000, 0.000000000000000000, 1.000000000000000000 ) ) ;
#8119 = CARTESIAN_POINT ( 'NONE',  ( -2.000000000000001776, 0.000000000000000000, 0.000000000000000000 ) ) ;
#8120 = CARTESIAN_POINT ( 'NONE',  ( 3.181980515339458471, 3.181980515339470461, 2.232096619617652273E-17 ) ) ;
#8121 = CARTESIAN_POINT ( 'NONE',  ( -2.042957248827969252, 4.009529358847651714, 13.43999999999999950 ) ) ;
#8122 = ORIENTED_EDGE ( 'NONE', *, *, #9791, .T. ) ;
#8123 = VECTOR ( 'NONE', #3044, 1000.000000000000000 ) ;
#8124 = CARTESIAN_POINT ( 'NONE',  ( -0.6146835312499998594, -11.93533689329915326, -1.177083334016129967 ) ) ;
#8125 = ADVANCED_FACE ( 'NONE', ( #7670 ), #4527, .F. ) ;
#8126 = EDGE_CURVE ( 'NONE', #5056, #5181, #6434, .T. ) ;
#8127 = CARTESIAN_POINT ( 'NONE',  ( -0.9046671180729963790, 5.711843387010016926, 5.179999999999999716 ) ) ;
#8128 = CARTESIAN_POINT ( 'NONE',  ( 22.43558391966725907, 3.750000000000000000, -12.00000000000000000 ) ) ;
#8129 = CONTEXT_DEPENDENT_SHAPE_REPRESENTATION ( #9611, #9798 ) ;
#8130 = LINE ( 'NONE', #866, #865 ) ;
#8131 = VECTOR ( 'NONE', #1547, 1000.000000000000000 ) ;
#8132 = DIRECTION ( 'NONE',  ( -0.000000000000000000, 1.000000000000000000, -0.000000000000000000 ) ) ;
#8133 = AXIS2_PLACEMENT_3D ( 'NONE', #3473, #6315, #1342 ) ;
#8134 = EDGE_CURVE ( 'NONE', #9850, #7675, #1702, .T. ) ;
#8135 = DIRECTION ( 'NONE',  ( -1.000000000000000000, 0.000000000000000000, 0.000000000000000000 ) ) ;
#8136 = LINE ( 'NONE', #9224, #3098 ) ;
#8137 = ORIENTED_EDGE ( 'NONE', *, *, #8140, .F. ) ;
#8138 = CARTESIAN_POINT ( 'NONE',  ( -4.049832306626335310, 1.963858260114700327, 2.956051716722023492 ) ) ;
#8139 = DIRECTION ( 'NONE',  ( -1.000000000000000000, -0.000000000000000000, -0.000000000000000000 ) ) ;
#8140 = EDGE_CURVE ( 'NONE', #6819, #6622, #8476, .T. ) ;
#8141 = VECTOR ( 'NONE', #1843, 1000.000000000000000 ) ;
#8142 = CARTESIAN_POINT ( 'NONE',  ( -3.244753828200538148, -3.119207202478392116, 6.003948283277975584 ) ) ;
#8143 = VECTOR ( 'NONE', #8705, 1000.000000000000000 ) ;
#8144 = CARTESIAN_POINT ( 'NONE',  ( 10.00000000000000000, 0.000000000000000000, 0.000000000000000000 ) ) ;
#8145 = VERTEX_POINT ( 'NONE', #2950 ) ;
#8146 = ORIENTED_EDGE ( 'NONE', *, *, #6334, .T. ) ;
#8147 = CARTESIAN_POINT ( 'NONE',  ( 10.00000000000000000, 52.93638525830372998, 8.843061888689529582 ) ) ;
#8148 = AXIS2_PLACEMENT_3D ( 'NONE', #3996, #7227, #8604 ) ;
#8149 = DIRECTION ( 'NONE',  ( -1.000000000000000000, -0.000000000000000000, -0.000000000000000000 ) ) ;
#8150 = ORIENTED_EDGE ( 'NONE', *, *, #628, .T. ) ;
#8151 = CARTESIAN_POINT ( 'NONE',  ( 3.181980515339458471, 3.181980515339470461, 3.651811961182260059E-17 ) ) ;
#8152 = AXIS2_PLACEMENT_3D ( 'NONE', #4890, #6476, #130 ) ;
#8153 = LINE ( 'NONE', #10441, #4059 ) ;
#8154 = EDGE_LOOP ( 'NONE', ( #7342, #8838, #4206, #2896 ) ) ;
#8155 = CARTESIAN_POINT ( 'NONE',  ( 0.8323763977770604061, -4.658724279160015413, 7.576051716722023599 ) ) ;
#8156 = VECTOR ( 'NONE', #7257, 1000.000000000000000 ) ;
#8157 = CONICAL_SURFACE ( 'NONE', #10219, 1.280000000000000027, 1.047197551196593857 ) ;
#8158 = ORIENTED_EDGE ( 'NONE', *, *, #10433, .T. ) ;
#8159 = VERTEX_POINT ( 'NONE', #504 ) ;
#8160 = VECTOR ( 'NONE', #2369, 1000.000000000000000 ) ;
#8161 = LINE ( 'NONE', #8210, #9926 ) ;
#8162 = DIRECTION ( 'NONE',  ( 1.156482317317871478E-16, -1.000000000000000000, -0.000000000000000000 ) ) ;
#8163 = ORIENTED_EDGE ( 'NONE', *, *, #387, .F. ) ;
#8164 = CARTESIAN_POINT ( 'NONE',  ( 5.152728359536493663, 2.625446233515533745, 2.939999999999999059 ) ) ;
#8165 = PLANE ( 'NONE',  #7669 ) ;
#8166 = CARTESIAN_POINT ( 'NONE',  ( -4.023224611898323033, 4.155232146225737111, 12.30394828327797718 ) ) ;
#8167 = VERTEX_POINT ( 'NONE', #458 ) ;
#8168 = CARTESIAN_POINT ( 'NONE',  ( -1.500000000000000000, -12.13397459621556607, -1.354166668032260157 ) ) ;
#8169 = ORIENTED_EDGE ( 'NONE', *, *, #1901, .T. ) ;
#8170 = PLANE ( 'NONE',  #2286 ) ;
#8171 = DIRECTION ( 'NONE',  ( -1.000000000000000000, 0.000000000000000000, 5.204170427930421283E-15 ) ) ;
#8172 = DIRECTION ( 'NONE',  ( -1.156482317317871478E-16, 1.000000000000000000, 0.000000000000000000 ) ) ;
#8173 = CARTESIAN_POINT ( 'NONE',  ( 0.000000000000000000, -13.00000000000000533, -3.000000000000000000 ) ) ;
#8174 = EDGE_CURVE ( 'NONE', #9192, #1286, #7798, .T. ) ;
#8175 = CARTESIAN_POINT ( 'NONE',  ( 1.229367062500000163, -13.00000000000000533, -2.843750000682796486 ) ) ;
#8176 = CARTESIAN_POINT ( 'NONE',  ( -3.969226411068985882, 2.122056237541205537, 3.763948283277976703 ) ) ;
#8177 = ORIENTED_EDGE ( 'NONE', *, *, #4450, .T. ) ;
#8178 = DIRECTION ( 'NONE',  ( 0.000000000000000000, 0.000000000000000000, 1.000000000000000000 ) ) ;
#8179 = CARTESIAN_POINT ( 'NONE',  ( -2.625446233515515981, -5.152728359536500768, 6.859999999999999432 ) ) ;
#8180 = PLANE ( 'NONE',  #6307 ) ;
#8181 = ITEM_DEFINED_TRANSFORMATION ( 'NONE', 'NONE', #4145,  #2101 ) ;
#8182 = CARTESIAN_POINT ( 'NONE',  ( 4.900535883036028828, -2.496947748567499126, 8.959999999999999076 ) ) ;
#8183 = CARTESIAN_POINT ( 'NONE',  ( 30.00000000000001066, -34.99999999999999289, 9.000000000000000000 ) ) ;
#8184 = EDGE_CURVE ( 'NONE', #376, #1802, #5374, .T. ) ;
#8185 = DIRECTION ( 'NONE',  ( -0.000000000000000000, -1.000000000000000000, -0.000000000000000000 ) ) ;
#8186 = EDGE_CURVE ( 'NONE', #9543, #8145, #7180, .T. ) ;
#8187 = DIRECTION ( 'NONE',  ( -1.000000000000000000, -0.000000000000000000, -0.000000000000000000 ) ) ;
#8188 = PRODUCT_DEFINITION_SHAPE ( 'NONE', 'NONE',  #10506 ) ;
#8189 = CARTESIAN_POINT ( 'NONE',  ( 3.000000000000002665, 3.367778697655221012E-16, -2.750000000000000000 ) ) ;
#8190 = CARTESIAN_POINT ( 'NONE',  ( 3.119207202478379681, 3.244753828200549695, 0.9960517167220231949 ) ) ;
#8191 = CARTESIAN_POINT ( 'NONE',  ( 3.535533905932731980, 3.535533905932744414, -8.174322470544786116E-18 ) ) ;
#8192 = CARTESIAN_POINT ( 'NONE',  ( -3.244753828200538148, -3.119207202478392116, 8.803948283277977183 ) ) ;
#8193 = VECTOR ( 'NONE', #9893, 1000.000000000000000 ) ;
#8194 = CARTESIAN_POINT ( 'NONE',  ( -26.99999999999998934, -32.00000000000000000, 5.999999999999999112 ) ) ;
#8195 = EDGE_LOOP ( 'NONE', ( #9205, #2, #3397, #8902 ) ) ;
#8196 = EDGE_LOOP ( 'NONE', ( #6347, #9272, #6331, #2063 ) ) ;
#8197 = ADVANCED_FACE ( 'NONE', ( #2364 ), #4799, .T. ) ;
#8198 = CARTESIAN_POINT ( 'NONE',  ( -31.74999999999995737, 0.000000000000000000, 0.000000000000000000 ) ) ;
#8199 = DIRECTION ( 'NONE',  ( -1.000000000000000000, -0.000000000000000000, -0.000000000000000000 ) ) ;
#8200 = VERTEX_POINT ( 'NONE', #8834 ) ;
#8201 = AXIS2_PLACEMENT_3D ( 'NONE', #2505, #68, #3346 ) ;
#8202 = FACE_BOUND ( 'NONE', #3427, .T. ) ;
#8203 = DIRECTION ( 'NONE',  ( 0.000000000000000000, -0.000000000000000000, 1.000000000000000000 ) ) ;
#8204 = ORIENTED_EDGE ( 'NONE', *, *, #4946, .T. ) ;
#8205 = CARTESIAN_POINT ( 'NONE',  ( -0.6162731882459178134, -4.458484982038665834, 4.916051716722023457 ) ) ;
#8206 = DIRECTION ( 'NONE',  ( -1.156482317317871478E-16, 1.000000000000000000, 0.000000000000000000 ) ) ;
#8207 = ORIENTED_EDGE ( 'NONE', *, *, #6468, .F. ) ;
#8208 = AXIS2_PLACEMENT_3D ( 'NONE', #8900, #6501, #6452 ) ;
#8209 = ORIENTED_EDGE ( 'NONE', *, *, #1171, .T. ) ;
#8210 = CARTESIAN_POINT ( 'NONE',  ( 0.000000000000000000, 0.000000000000000000, -12.00000000000000000 ) ) ;
#8211 = FACE_OUTER_BOUND ( 'NONE', #5175, .T. ) ;
#8212 = EDGE_LOOP ( 'NONE', ( #4767, #6509, #770, #3214 ) ) ;
#8213 = CARTESIAN_POINT ( 'NONE',  ( -5.432285873273256627, -0.8603895577212797852, 1.679999999999999938 ) ) ;
#8214 = CARTESIAN_POINT ( 'NONE',  ( 4.900535883036028828, -2.496947748567499126, 3.359999999999999876 ) ) ;
#8215 =( GEOMETRIC_REPRESENTATION_CONTEXT ( 3 ) GLOBAL_UNCERTAINTY_ASSIGNED_CONTEXT ( ( #8037 ) ) GLOBAL_UNIT_ASSIGNED_CONTEXT ( ( #5811, #5962, #4278 ) ) REPRESENTATION_CONTEXT ( 'NONE', 'WORKASPACE' ) );
#8216 = CARTESIAN_POINT ( 'NONE',  ( -5.446173322633801384, -0.7727076532861678615, 11.88394828327797548 ) ) ;
#8217 = ORIENTED_EDGE ( 'NONE', *, *, #6947, .T. ) ;
#8218 = CARTESIAN_POINT ( 'NONE',  ( 1.229367062500000163, -13.00000000000000533, 0.2812499993172035695 ) ) ;
#8219 = VECTOR ( 'NONE', #5029, 1000.000000000000000 ) ;
#8220 =( LENGTH_UNIT ( ) NAMED_UNIT ( * ) SI_UNIT ( .MILLI., .METRE. ) );
#8221 = VERTEX_POINT ( 'NONE', #3002 ) ;
#8222 = DIRECTION ( 'NONE',  ( 0.3420201433256627732, -0.9396926207859105373, 0.000000000000000000 ) ) ;
#8223 = CARTESIAN_POINT ( 'NONE',  ( 0.000000000000000000, -13.00000000000000533, -3.000000000000000000 ) ) ;
#8224 = PLANE ( 'NONE',  #9665 ) ;
#8225 = VERTEX_POINT ( 'NONE', #613 ) ;
#8226 = FACE_OUTER_BOUND ( 'NONE', #5551, .T. ) ;
#8227 = AXIS2_PLACEMENT_3D ( 'NONE', #6652, #7460, #5903 ) ;
#8228 = CARTESIAN_POINT ( 'NONE',  ( -0.6146835312499998594, -11.93533689329915326, -2.177083334016129967 ) ) ;
#8229 = EDGE_CURVE ( 'NONE', #789, #7999, #10437, .T. ) ;
#8230 = CARTESIAN_POINT ( 'NONE',  ( 2.231261971483764484, 4.173491630687871101, 1.663948283277976392 ) ) ;
#8231 = ORIENTED_EDGE ( 'NONE', *, *, #9938, .T. ) ;
#8232 = CARTESIAN_POINT ( 'NONE',  ( -0.6146835312500006365, -14.06466310670085562, -0.01041666734946352160 ) ) ;
#8233 = CARTESIAN_POINT ( 'NONE',  ( -3.889087296526005044, -3.889087296526019255, 4.200000000000000178 ) ) ;
#8234 = DIRECTION ( 'NONE',  ( -1.000000000000000000, -0.000000000000000000, -0.000000000000000000 ) ) ;
#8235 = CIRCLE ( 'NONE', #9421, 2.000000000000000000 ) ;
#8236 = EDGE_CURVE ( 'NONE', #1737, #7025, #6254, .T. ) ;
#8237 = ITEM_DEFINED_TRANSFORMATION ( 'NONE', 'NONE', #3639,  #2101 ) ;
#8238 = CARTESIAN_POINT ( 'NONE',  ( 4.089228379062037178, -4.089228379062022967, 9.099999999999996092 ) ) ;
#8239 = VECTOR ( 'NONE', #3039, 1000.000000000000000 ) ;
#8240 = CARTESIAN_POINT ( 'NONE',  ( 8.000000000000001776, -6.700937042937042065, -2.183447440113260196 ) ) ;
#8241 = MANIFOLD_SOLID_BREP ( 'Sweep1', #4551 ) ;
#8242 = DIRECTION ( 'NONE',  ( 0.000000000000000000, 0.000000000000000000, -1.000000000000000000 ) ) ;
#8243 = DIRECTION ( 'NONE',  ( 0.000000000000000000, 0.000000000000000000, 1.000000000000000000 ) ) ;
#8244 = CARTESIAN_POINT ( 'NONE',  ( 2.064922774268895811, 4.258245684917319807, 3.656051716722022782 ) ) ;
#8245 = PLANE ( 'NONE',  #4573 ) ;
#8246 = CARTESIAN_POINT ( 'NONE',  ( -3.279728542977953687, 3.411736077305369541, 9.503948283277974696 ) ) ;
#8247 = EDGE_CURVE ( 'NONE', #909, #8622, #1574, .T. ) ;
#8248 = DIRECTION ( 'NONE',  ( -0.000000000000000000, -1.000000000000000000, -0.000000000000000000 ) ) ;
#8249 = EDGE_CURVE ( 'NONE', #8955, #5062, #4331, .T. ) ;
#8250 = VERTEX_POINT ( 'NONE', #4008 ) ;
#8251 = CARTESIAN_POINT ( 'NONE',  ( 4.940838830814703542, -2.417848759854246410, 1.556051716722023581 ) ) ;
#8252 = FACE_OUTER_BOUND ( 'NONE', #9489, .T. ) ;
#8253 = CYLINDRICAL_SURFACE ( 'NONE', #6770, 8.500000000000000000 ) ;
#8254 = ORIENTED_EDGE ( 'NONE', *, *, #7743, .F. ) ;
#8255 = CARTESIAN_POINT ( 'NONE',  ( -2.000000000000000000, -7.851777359433979697, -3.255701506262516087 ) ) ;
#8256 = ORIENTED_EDGE ( 'NONE', *, *, #4869, .T. ) ;
#8257 = CARTESIAN_POINT ( 'NONE',  ( -2.122056237541221968, 3.969226411068977889, 11.63605171672202232 ) ) ;
#8258 = AXIS2_PLACEMENT_3D ( 'NONE', #9989, #4347, #7588 ) ;
#8259 = ADVANCED_FACE ( 'NONE', ( #9472 ), #7237, .T. ) ;
#8260 = DIRECTION ( 'NONE',  ( -1.000000000000000000, 0.000000000000000000, -0.000000000000000000 ) ) ;
#8261 = ORIENTED_EDGE ( 'NONE', *, *, #8093, .F. ) ;
#8262 =( NAMED_UNIT ( * ) PLANE_ANGLE_UNIT ( ) SI_UNIT ( $, .RADIAN. ) );
#8263 = ORIENTED_EDGE ( 'NONE', *, *, #10127, .F. ) ;
#8264 = LINE ( 'NONE', #990, #3306 ) ;
#8265 =( NAMED_UNIT ( * ) PLANE_ANGLE_UNIT ( ) SI_UNIT ( $, .RADIAN. ) );
#8266 = VERTEX_POINT ( 'NONE', #4685 ) ;
#8267 = CARTESIAN_POINT ( 'NONE',  ( -5.110351332421769754, -2.708615832122969191, 2.536051716722023119 ) ) ;
#8268 = CARTESIAN_POINT ( 'NONE',  ( -5.152728359536494551, -2.625446233515535077, 1.540000000000000036 ) ) ;
#8269 = CARTESIAN_POINT ( 'NONE',  ( -0.8603895577212598011, -5.432285873273260179, 3.919999999999999929 ) ) ;
#8270 = VERTEX_POINT ( 'NONE', #7929 ) ;
#8271 = CARTESIAN_POINT ( 'NONE',  ( 8.692241771943169307E-17, -11.58044919106553294, -0.5937500006827968191 ) ) ;
#8272 = EDGE_CURVE ( 'NONE', #7306, #2835, #8092, .T. ) ;
#8273 =( NAMED_UNIT ( * ) SI_UNIT ( $, .STERADIAN. ) SOLID_ANGLE_UNIT ( ) );
#8274 = VERTEX_POINT ( 'NONE', #6325 ) ;
#8275 = DIRECTION ( 'NONE',  ( -1.000000000000000000, -0.000000000000000000, 0.000000000000000000 ) ) ;
#8276 = PLANE ( 'NONE',  #2047 ) ;
#8277 = LINE ( 'NONE', #9117, #6246 ) ;
#8278 = ORIENTED_EDGE ( 'NONE', *, *, #2039, .T. ) ;
#8279 = LINE ( 'NONE', #4981, #7091 ) ;
#8280 = CARTESIAN_POINT ( 'NONE',  ( -1.229367062500000163, -13.00000000000000533, -1.093750000682796486 ) ) ;
#8281 = CARTESIAN_POINT ( 'NONE',  ( 3.969226411068985882, -2.122056237541205981, -0.4360517167220233636 ) ) ;
#8282 = ORIENTED_EDGE ( 'NONE', *, *, #6981, .T. ) ;
#8283 = CARTESIAN_POINT ( 'NONE',  ( 16.98057649071655817, 6.025400000000000311, 0.000000000000000000 ) ) ;
#8284 =( BOUNDED_CURVE ( )  B_SPLINE_CURVE ( 2, ( #3865, #10353, #8749, #8070, #4029, #1600, #9557 ),
 .UNSPECIFIED., .F., .T. ) 
 B_SPLINE_CURVE_WITH_KNOTS ( ( 3, 2, 2, 3 ),
 ( 0.2499999999999999167, 0.2777777777777777346, 0.3055555555555555802, 0.3333333333333333148 ),
 .UNSPECIFIED. ) 
 CURVE ( )  GEOMETRIC_REPRESENTATION_ITEM ( )  RATIONAL_B_SPLINE_CURVE ( ( 1.000000000000000222, 0.8660254037844382635, 1.000000000000000000, 0.8660254037844387076, 1.000000000000000000, 0.8660254037844387076, 1.000000000000000000 ) ) 
 REPRESENTATION_ITEM ( '' )  );
#8285 = CARTESIAN_POINT ( 'NONE',  ( -4.089228379062038066, 4.089228379062021190, 4.900000000000000355 ) ) ;
#8286 = DIRECTION ( 'NONE',  ( 0.000000000000000000, -0.5000000000000009992, -0.8660254037844380415 ) ) ;
#8287 = CARTESIAN_POINT ( 'NONE',  ( 2.496947748567516889, -4.900535883036019946, 9.240000000000000213 ) ) ;
#8288 = FACE_OUTER_BOUND ( 'NONE', #9265, .T. ) ;
#8289 = DIRECTION ( 'NONE',  ( 0.000000000000000000, 0.000000000000000000, 1.000000000000000000 ) ) ;
#8290 = CIRCLE ( 'NONE', #3869, 1.500000000000000222 ) ;
#8291 = CYLINDRICAL_SURFACE ( 'NONE', #5984, 3.000000000000000000 ) ;
#8292 = CARTESIAN_POINT ( 'NONE',  ( -5.726445515403654873, 0.8124729078101847746, 14.01605171672202310 ) ) ;
#8293 = EDGE_CURVE ( 'NONE', #6113, #3693, #9584, .T. ) ;
#8294 = CARTESIAN_POINT ( 'NONE',  ( -0.6146835312499998594, -11.93533689329915326, -1.552083334016129967 ) ) ;
#8295 = CARTESIAN_POINT ( 'NONE',  ( -0.7916369971161423269, -4.430710083317576320, 5.723948283277976223 ) ) ;
#8296 = CARTESIAN_POINT ( 'NONE',  ( -2.000000000000000000, -6.700937042937042065, -2.183447440113260196 ) ) ;
#8297 = VERTEX_POINT ( 'NONE', #4742 ) ;
#8298 = CIRCLE ( 'NONE', #3206, 6.248999999999999666 ) ;
#8299 = CARTESIAN_POINT ( 'NONE',  ( -5.726445515403654873, 0.8124729078101847746, 5.616051716722022746 ) ) ;
#8300 = DIRECTION ( 'NONE',  ( 0.000000000000000000, 0.000000000000000000, -1.000000000000000000 ) ) ;
#8301 = CARTESIAN_POINT ( 'NONE',  ( 1.263368396766194612, -10.00000000000000000, -12.00000000000000000 ) ) ;
#8302 = ORIENTED_EDGE ( 'NONE', *, *, #10395, .F. ) ;
#8303 = CIRCLE ( 'NONE', #337, 3.000000000000000000 ) ;
#8304 = EDGE_CURVE ( 'NONE', #2001, #1747, #7989, .T. ) ;
#8305 = LINE ( 'NONE', #1036, #6068 ) ;
#8306 = DIRECTION ( 'NONE',  ( -0.3420201433256627732, 0.9396926207859105373, 0.000000000000000000 ) ) ;
#8307 = ORIENTED_EDGE ( 'NONE', *, *, #5401, .T. ) ;
#8308 = COLOUR_RGB ( '', 0.08235294, 0.09019608, 0.10196078) ;
#8309 = CARTESIAN_POINT ( 'NONE',  ( 2.122056237541221524, -3.969226411068978777, 13.03605171672202090 ) ) ;
#8310 = CARTESIAN_POINT ( 'NONE',  ( 1.229367062499999719, -13.70977540446724063, -2.385416667349463005 ) ) ;
#8311 = EDGE_LOOP ( 'NONE', ( #6000, #9137, #659, #3906 ) ) ;
#8312 = DIRECTION ( 'NONE',  ( 0.000000000000000000, 1.000000000000000000, 0.000000000000000000 ) ) ;
#8313 = AXIS2_PLACEMENT_3D ( 'NONE', #6754, #9208, #1947 ) ;
#8314 = ORIENTED_EDGE ( 'NONE', *, *, #8066, .F. ) ;
#8315 = CARTESIAN_POINT ( 'NONE',  ( 1.500000000000000222, -13.00000000000000533, -3.000000000000000000 ) ) ;
#8316 = CIRCLE ( 'NONE', #9675, 3.000000000000000000 ) ;
#8317 = PLANE ( 'NONE',  #2382 ) ;
#8318 = ORIENTED_EDGE ( 'NONE', *, *, #3635, .T. ) ;
#8319 = ADVANCED_FACE ( 'NONE', ( #1672 ), #5052, .F. ) ;
#8320 = CARTESIAN_POINT ( 'NONE',  ( 4.155232146225751322, -4.023224611898307934, 1.696051716722023484 ) ) ;
#8321 = ADVANCED_FACE ( 'NONE', ( #4256 ), #5108, .T. ) ;
#8322 = CARTESIAN_POINT ( 'NONE',  ( 0.8603895577212593571, 5.432285873273261068, 8.119999999999999218 ) ) ;
#8323 = AXIS2_PLACEMENT_3D ( 'NONE', #10117, #1199, #2051 ) ;
#8324 = CARTESIAN_POINT ( 'NONE',  ( 4.900535883036028828, -2.496947748567499126, 8.959999999999999076 ) ) ;
#8325 = ORIENTED_EDGE ( 'NONE', *, *, #4279, .F. ) ;
#8326 = AXIS2_PLACEMENT_3D ( 'NONE', #979, #1034, #2675 ) ;
#8327 = CARTESIAN_POINT ( 'NONE',  ( 1.229367062499999719, -13.70977540446724063, -1.260416667349463449 ) ) ;
#8328 = PRESENTATION_STYLE_ASSIGNMENT (( #5075 ) ) ;
#8329 = VERTEX_POINT ( 'NONE', #6642 ) ;
#8330 = CIRCLE ( 'NONE', #5096, 3.000000000000000000 ) ;
#8331 = CARTESIAN_POINT ( 'NONE',  ( 8.000000000000001776, -7.009698679648282749, -0.7308381473897593850 ) ) ;
#8332 = CYLINDRICAL_SURFACE ( 'NONE', #6929, 1.500000000000000222 ) ;
#8333 = VERTEX_POINT ( 'NONE', #8301 ) ;
#8334 = EDGE_CURVE ( 'NONE', #10028, #6306, #2473, .T. ) ;
#8335 = DIRECTION ( 'NONE',  ( -1.000000000000000000, -0.000000000000000000, -0.000000000000000000 ) ) ;
#8336 = CARTESIAN_POINT ( 'NONE',  ( 0.6146835312500001924, -11.93533689329915326, -0.7604166673494633377 ) ) ;
#8337 = CARTESIAN_POINT ( 'NONE',  ( 0.7916369971161419938, 4.430710083317576320, 9.923948283277976401 ) ) ;
#8338 = ORIENTED_EDGE ( 'NONE', *, *, #7005, .F. ) ;
#8339 = DIRECTION ( 'NONE',  ( -1.000000000000000000, 0.000000000000000000, 0.000000000000000000 ) ) ;
#8340 = CARTESIAN_POINT ( 'NONE',  ( 30.00000000000001066, -34.99999999999999289, 9.000000000000000000 ) ) ;
#8341 = FACE_OUTER_BOUND ( 'NONE', #2479, .T. ) ;
#8342 = CARTESIAN_POINT ( 'NONE',  ( -0.9046671180729962680, 5.711843387010016926, 5.179999999999999716 ) ) ;
#8343 = LINE ( 'NONE', #7538, #7552 ) ;
#8344 = FACE_OUTER_BOUND ( 'NONE', #1310, .T. ) ;
#8345 = DIRECTION ( 'NONE',  ( 0.000000000000000000, -0.000000000000000000, -1.000000000000000000 ) ) ;
#8346 = CARTESIAN_POINT ( 'NONE',  ( -3.119207202478379681, -3.244753828200550139, 7.996051716722022640 ) ) ;
#8347 = SHAPE_REPRESENTATION ( 'jaw_ISO - Spur gear 1M 15T 20PA 8FW ---S15A75H50L4.0N', ( #2101 ), #5648 ) ;
#8348 = DIRECTION ( 'NONE',  ( 0.000000000000000000, 0.000000000000000000, -1.000000000000000000 ) ) ;
#8349 = CARTESIAN_POINT ( 'NONE',  ( 3.969226411068985882, -2.122056237541205981, 2.363948283277975904 ) ) ;
#8350 = CARTESIAN_POINT ( 'NONE',  ( -2.607672531582950546E-16, -14.41955080893447416, -2.343750000682796042 ) ) ;
#8351 = EDGE_LOOP ( 'NONE', ( #5600, #6133, #4723, #5443 ) ) ;
#8352 = CARTESIAN_POINT ( 'NONE',  ( -5.726445515403654873, 0.8124729078101847746, 2.816051716722022924 ) ) ;
#8353 = DIRECTION ( 'NONE',  ( -1.000000000000000000, 0.000000000000000000, -0.000000000000000000 ) ) ;
#8354 = CARTESIAN_POINT ( 'NONE',  ( -26.99999999999998934, -13.00000000000000533, 0.000000000000000000 ) ) ;
#8355 = VERTEX_POINT ( 'NONE', #9897 ) ;
#8356 = LINE ( 'NONE', #5110, #2024 ) ;
#8357 = CIRCLE ( 'NONE', #3439, 3.000000000000000000 ) ;
#8358 = DIRECTION ( 'NONE',  ( 0.000000000000000000, 0.000000000000000000, 1.000000000000000000 ) ) ;
#8359 = CARTESIAN_POINT ( 'NONE',  ( 2.064922774268895811, 4.258245684917319807, 6.456051716722022604 ) ) ;
#8360 = CARTESIAN_POINT ( 'NONE',  ( -29.99999999999998934, -35.00000000000000000, 9.000000000000000000 ) ) ;
#8361 = ORIENTED_EDGE ( 'NONE', *, *, #8426, .F. ) ;
#8362 = PRESENTATION_STYLE_ASSIGNMENT (( #6702 ) ) ;
#8363 = ADVANCED_FACE ( 'NONE', ( #5889 ), #8932, .T. ) ;
#8364 = ORIENTED_EDGE ( 'NONE', *, *, #8829, .T. ) ;
#8365 = AXIS2_PLACEMENT_3D ( 'NONE', #2669, #1025, #2570 ) ;
#8366 = LINE ( 'NONE', #10164, #3489 ) ;
#8367 = ORIENTED_EDGE ( 'NONE', *, *, #6786, .F. ) ;
#8368 = CARTESIAN_POINT ( 'NONE',  ( -5.152728359536494551, -2.625446233515535077, 9.939999999999994174 ) ) ;
#8369 = DIRECTION ( 'NONE',  ( 0.000000000000000000, 0.000000000000000000, -1.000000000000000000 ) ) ;
#8370 = CARTESIAN_POINT ( 'NONE',  ( 0.8603895577212593571, 5.432285873273261068, 8.119999999999999218 ) ) ;
#8371 = VERTEX_POINT ( 'NONE', #5843 ) ;
#8372 = CARTESIAN_POINT ( 'NONE',  ( -0.6146835312500006365, -14.06466310670085562, -1.385416667349463227 ) ) ;
#8373 = VECTOR ( 'NONE', #6085, 1000.000000000000000 ) ;
#8374 = EDGE_CURVE ( 'NONE', #1802, #7779, #823, .T. ) ;
#8375 = ADVANCED_FACE ( 'NONE', ( #5688 ), #2520, .F. ) ;
#8376 = EDGE_LOOP ( 'NONE', ( #8672, #7314, #3291, #4589 ) ) ;
#8377 = CARTESIAN_POINT ( 'NONE',  ( 8.000000000000001776, -6.106419733534973915, -3.518755179752866447 ) ) ;
#8378 = CARTESIAN_POINT ( 'NONE',  ( 0.000000000000000000, -13.00000000000000533, -3.000000000000000000 ) ) ;
#8379 = VERTEX_POINT ( 'NONE', #8989 ) ;
#8380 = CARTESIAN_POINT ( 'NONE',  ( 12.12193523033274545, 3.750000000000000000, -12.00000000000000000 ) ) ;
#8381 = FACE_OUTER_BOUND ( 'NONE', #8789, .T. ) ;
#8382 = CARTESIAN_POINT ( 'NONE',  ( 1.229367062500000163, -12.29022459553277002, -0.3020833340161301339 ) ) ;
#8383 = CARTESIAN_POINT ( 'NONE',  ( -1.963858260114716980, 4.049832306626327316, 6.843948283277976330 ) ) ;
#8384 = VERTEX_POINT ( 'NONE', #191 ) ;
#8385 = VECTOR ( 'NONE', #6296, 1000.000000000000000 ) ;
#8386 = CARTESIAN_POINT ( 'NONE',  ( 10.00000000000000000, -7.673322273190701814, -3.656518192455153748 ) ) ;
#8387 = CARTESIAN_POINT ( 'NONE',  ( -2.625446233515515981, -5.152728359536500768, 9.659999999999994813 ) ) ;
#8388 = AXIS2_PLACEMENT_3D ( 'NONE', #1840, #2836, #9152 ) ;
#8389 = EDGE_CURVE ( 'NONE', #138, #1592, #930, .T. ) ;
#8390 = CARTESIAN_POINT ( 'NONE',  ( 10.68814634676619413, -10.00000000000000000, -12.00000000000000000 ) ) ;
#8391 = CARTESIAN_POINT ( 'NONE',  ( -4.900535883036028828, 2.496947748567499126, 10.35999999999999943 ) ) ;
#8392 = CIRCLE ( 'NONE', #3479, 2.000000000000003553 ) ;
#8393 = LINE ( 'NONE', #10043, #2481 ) ;
#8394 = CARTESIAN_POINT ( 'NONE',  ( -1.500000000000000222, -13.00000000000000533, -1.812500001365593416 ) ) ;
#8395 = CARTESIAN_POINT ( 'NONE',  ( 22.43558391966725907, 3.750000000000000000, 0.000000000000000000 ) ) ;
#8396 = CARTESIAN_POINT ( 'NONE',  ( 2.122056237541221524, -3.969226411068978777, 10.23605171672202374 ) ) ;
#8397 = CARTESIAN_POINT ( 'NONE',  ( 0.6146835312500001924, -11.93533689329915326, -2.635416667349463449 ) ) ;
#8398 = VECTOR ( 'NONE', #3853, 1000.000000000000000 ) ;
#8399 = CARTESIAN_POINT ( 'NONE',  ( 3.951860609387084722, 3.826313983664940022, -0.9960517167220231949 ) ) ;
#8400 = EDGE_CURVE ( 'NONE', #9902, #4905, #6262, .T. ) ;
#8401 = CARTESIAN_POINT ( 'NONE',  ( -1.229367062500000163, -12.29022459553277002, -1.510416667349463227 ) ) ;
#8402 = AXIS2_PLACEMENT_3D ( 'NONE', #8975, #8135, #916 ) ;
#8403 = VERTEX_POINT ( 'NONE', #7345 ) ;
#8404 = CARTESIAN_POINT ( 'NONE',  ( -4.940838830814703542, 2.417848759854245078, 5.756051716722022427 ) ) ;
#8405 = DIRECTION ( 'NONE',  ( 1.000000000000000000, -0.000000000000000000, -0.000000000000000000 ) ) ;
#8406 = VECTOR ( 'NONE', #4194, 1000.000000000000000 ) ;
#8407 = CARTESIAN_POINT ( 'NONE',  ( -1.500000000000000222, -13.00000000000000533, -3.000000000000000000 ) ) ;
#8408 = ORIENTED_EDGE ( 'NONE', *, *, #5357, .F. ) ;
#8409 = CIRCLE ( 'NONE', #2985, 3.000000000000000000 ) ;
#8410 = CARTESIAN_POINT ( 'NONE',  ( 4.444597532678119300, 0.7039550926810472786, 11.47999999999999865 ) ) ;
#8411 = SURFACE_STYLE_USAGE ( .BOTH. , #2042 ) ;
#8412 = CARTESIAN_POINT ( 'NONE',  ( 4.215868657802586128, 2.148092372876346801, 0.1400000000000000411 ) ) ;
#8413 = DIRECTION ( 'NONE',  ( 0.000000000000000000, -0.000000000000000000, 1.000000000000000000 ) ) ;
#8414 = ORIENTED_EDGE ( 'NONE', *, *, #9786, .T. ) ;
#8415 = DIRECTION ( 'NONE',  ( -1.000000000000000000, 0.000000000000000000, 0.000000000000000000 ) ) ;
#8416 = ORIENTED_EDGE ( 'NONE', *, *, #9000, .T. ) ;
#8417 = ADVANCED_FACE ( 'NONE', ( #7289 ), #2626, .F. ) ;
#8418 = LINE ( 'NONE', #10063, #9236 ) ;
#8419 = CARTESIAN_POINT ( 'NONE',  ( 1.364683531250000303, -13.00000000000000533, -2.921875000341398465 ) ) ;
#8420 = ORIENTED_EDGE ( 'NONE', *, *, #787, .T. ) ;
#8421 = CARTESIAN_POINT ( 'NONE',  ( -5.432285873273256627, -0.8603895577212797852, 12.87999999999999901 ) ) ;
#8422 = CARTESIAN_POINT ( 'NONE',  ( -5.711843387010018702, 0.9046671180729746187, 4.620000000000000107 ) ) ;
#8423 = CARTESIAN_POINT ( 'NONE',  ( -2.496947748567517333, 4.900535883036019058, 5.039999999999999147 ) ) ;
#8424 = VERTEX_POINT ( 'NONE', #4053 ) ;
#8425 = CARTESIAN_POINT ( 'NONE',  ( -1.229367062500000385, -13.70977540446723886, 0.07291666598387017140 ) ) ;
#8426 = EDGE_CURVE ( 'NONE', #3837, #2653, #9501, .T. ) ;
#8427 =( NAMED_UNIT ( * ) SI_UNIT ( $, .STERADIAN. ) SOLID_ANGLE_UNIT ( ) );
#8428 = EDGE_LOOP ( 'NONE', ( #2349, #7225, #7663, #7968, #7656, #3800, #2630, #10221, #2831, #7836, #7620, #3859, #6322, #7718, #2967 ) ) ;
#8429 = CARTESIAN_POINT ( 'NONE',  ( 30.00000000000001066, -25.00000000000000000, 1.999999999999997780 ) ) ;
#8430 = LINE ( 'NONE', #7735, #2704 ) ;
#8431 = ORIENTED_EDGE ( 'NONE', *, *, #6480, .T. ) ;
#8432 = CARTESIAN_POINT ( 'NONE',  ( 21.54671318033274829, 3.750000000000000000, -12.00000000000000000 ) ) ;
#8433 = DIRECTION ( 'NONE',  ( -1.156482317317871478E-16, 1.000000000000000000, 0.000000000000000000 ) ) ;
#8434 = CARTESIAN_POINT ( 'NONE',  ( -0.6146835312500006365, -14.06466310670085562, -0.01041666734946352160 ) ) ;
#8435 = CARTESIAN_POINT ( 'NONE',  ( 5.697241258616385196, -0.9968613283357656840, -0.5760517167220230439 ) ) ;
#8436 = ORIENTED_EDGE ( 'NONE', *, *, #4165, .F. ) ;
#8437 = CARTESIAN_POINT ( 'NONE',  ( 21.54671318033274829, 3.750000000000000000, -12.00000000000000000 ) ) ;
#8438 = CARTESIAN_POINT ( 'NONE',  ( 2.625446233515515537, 5.152728359536502545, 11.05999999999999872 ) ) ;
#8439 = CARTESIAN_POINT ( 'NONE',  ( -5.999999999999999112, -27.00000000000000711, 3.000000000000000000 ) ) ;
#8440 = DIRECTION ( 'NONE',  ( 1.000000000000000000, 0.000000000000000000, 0.000000000000000000 ) ) ;
#8441 = FACE_BOUND ( 'NONE', #2585, .T. ) ;
#8442 = LINE ( 'NONE', #6033, #7038 ) ;
#8443 = FACE_OUTER_BOUND ( 'NONE', #2845, .T. ) ;
#8444 = CARTESIAN_POINT ( 'NONE',  ( 0.6162731882459174804, 4.458484982038668498, 9.116051716722020970 ) ) ;
#8445 = ADVANCED_FACE ( 'NONE', ( #6487 ), #3314, .T. ) ;
#8446 = EDGE_CURVE ( 'NONE', #4422, #5902, #190, .T. ) ;
#8447 = CYLINDRICAL_SURFACE ( 'NONE', #516, 2.000000000000001776 ) ;
#8448 = CARTESIAN_POINT ( 'NONE',  ( 2.417848759854264618, -4.940838830814695548, -0.1560517167220233370 ) ) ;
#8449 = CARTESIAN_POINT ( 'NONE',  ( 0.6146835312500001924, -11.93533689329915326, -0.6354166673494632267 ) ) ;
#8450 = VERTEX_POINT ( 'NONE', #5009 ) ;
#8451 = CARTESIAN_POINT ( 'NONE',  ( 0.9968613283357860011, -5.697241258616382531, 4.776051716722021112 ) ) ;
#8452 = CARTESIAN_POINT ( 'NONE',  ( 7.054542135639013677E-15, -28.99999999999999289, 0.000000000000000000 ) ) ;
#8453 = CARTESIAN_POINT ( 'NONE',  ( 20.11292429676619520, -10.00000000000000000, -12.00000000000000000 ) ) ;
#8454 = ORIENTED_EDGE ( 'NONE', *, *, #10108, .F. ) ;
#8455 = EDGE_CURVE ( 'NONE', #6381, #2302, #2575, .T. ) ;
#8456 = CARTESIAN_POINT ( 'NONE',  ( -0.7401821875142703400, 4.673326407553649808, 10.77999999999999936 ) ) ;
#8457 = LINE ( 'NONE', #1189, #341 ) ;
#8458 = CARTESIAN_POINT ( 'NONE',  ( 2.064922774268895811, 4.258245684917319807, 14.85605171672202296 ) ) ;
#8459 = AXIS2_PLACEMENT_3D ( 'NONE', #7084, #4761, #3913 ) ;
#8460 = CARTESIAN_POINT ( 'NONE',  ( 1.229367062500000163, -13.00000000000000533, -0.3437500006827965970 ) ) ;
#8461 = ORIENTED_EDGE ( 'NONE', *, *, #1708, .F. ) ;
#8462 = CARTESIAN_POINT ( 'NONE',  ( 0.000000000000000000, 0.000000000000000000, 0.000000000000000000 ) ) ;
#8463 = VECTOR ( 'NONE', #4997, 1000.000000000000000 ) ;
#8464 = ORIENTED_EDGE ( 'NONE', *, *, #5687, .T. ) ;
#8465 = FACE_OUTER_BOUND ( 'NONE', #3842, .T. ) ;
#8466 = CARTESIAN_POINT ( 'NONE',  ( 14.43535000928344481, 6.025400000000000311, -12.00000000000000000 ) ) ;
#8467 = AXIS2_PLACEMENT_3D ( 'NONE', #9663, #8014, #9769 ) ;
#8468 = CARTESIAN_POINT ( 'NONE',  ( 25.57717656966725883, 3.750000000000000000, -12.00000000000000000 ) ) ;
#8469 = ORIENTED_EDGE ( 'NONE', *, *, #5557, .T. ) ;
#8470 = STYLED_ITEM ( 'NONE', ( #1294 ), #4775 ) ;
#8471 = CARTESIAN_POINT ( 'NONE',  ( 4.089228379062037178, -4.089228379062022967, 11.90000000000000036 ) ) ;
#8472 = CARTESIAN_POINT ( 'NONE',  ( 0.8603895577212593571, 5.432285873273261068, 10.91999999999999993 ) ) ;
#8473 = CARTESIAN_POINT ( 'NONE',  ( 2.496947748567516889, -4.900535883036019946, 9.240000000000000213 ) ) ;
#8474 = EDGE_LOOP ( 'NONE', ( #5743, #7512, #5839, #6170 ) ) ;
#8475 = ADVANCED_FACE ( 'NONE', ( #1780 ), #8253, .T. ) ;
#8476 = CIRCLE ( 'NONE', #7105, 2.000000000000001776 ) ;
#8477 = AXIS2_PLACEMENT_3D ( 'NONE', #7846, #8802, #535 ) ;
#8478 = EDGE_LOOP ( 'NONE', ( #1988, #9920, #6276, #6057 ) ) ;
#8479 = CARTESIAN_POINT ( 'NONE',  ( -2.000000000000015987, 35.00000000000000000, -3.999999999999988898 ) ) ;
#8480 = CARTESIAN_POINT ( 'NONE',  ( 0.000000000000000000, -13.00000000000000533, -3.000000000000000000 ) ) ;
#8481 = ORIENTED_EDGE ( 'NONE', *, *, #2159, .F. ) ;
#8482 = FACE_OUTER_BOUND ( 'NONE', #5447, .T. ) ;
#8483 = VECTOR ( 'NONE', #5207, 1000.000000000000000 ) ;
#8484 = DIRECTION ( 'NONE',  ( -0.000000000000000000, 1.000000000000000000, 0.000000000000000000 ) ) ;
#8485 = DIRECTION ( 'NONE',  ( 0.000000000000000000, 0.000000000000000000, 1.000000000000000000 ) ) ;
#8486 = CARTESIAN_POINT ( 'NONE',  ( 3.279728542977952799, -3.411736077305369541, 8.103948283277974340 ) ) ;
#8487 = ORIENTED_EDGE ( 'NONE', *, *, #940, .T. ) ;
#8488 = CARTESIAN_POINT ( 'NONE',  ( 13.01080596966725622, 3.750000000000000000, -12.00000000000000000 ) ) ;
#8489 = CARTESIAN_POINT ( 'NONE',  ( 4.414205890716556446, -10.02539999999999942, -12.00000000000000000 ) ) ;
#8490 = VECTOR ( 'NONE', #2989, 1000.000000000000000 ) ;
#8491 = CARTESIAN_POINT ( 'NONE',  ( 4.000000000000000888, -8.497168642645963388, -0.2193742428685764301 ) ) ;
#8492 = CARTESIAN_POINT ( 'NONE',  ( -1.500000000000000222, -13.00000000000000533, -2.750000000000000000 ) ) ;
#8493 = EDGE_CURVE ( 'NONE', #1396, #4686, #8507, .T. ) ;
#8494 = FACE_OUTER_BOUND ( 'NONE', #8929, .T. ) ;
#8495 = CARTESIAN_POINT ( 'NONE',  ( 9.000000000000000000, 19.99999999999999645, 13.00000000000000000 ) ) ;
#8496 = CARTESIAN_POINT ( 'NONE',  ( -29.99999999999998934, 0.000000000000000000, 1.599999999999998979 ) ) ;
#8497 = CARTESIAN_POINT ( 'NONE',  ( -3.411736077305382420, 3.279728542977939476, 14.29605171672202424 ) ) ;
#8498 = CARTESIAN_POINT ( 'NONE',  ( 0.6146835312499993043, -14.06466310670085562, -0.8020833340161299674 ) ) ;
#8499 = CARTESIAN_POINT ( 'NONE',  ( -5.195105386651219348, -2.542276634908102295, 0.5439482832779766186 ) ) ;
#8500 = CARTESIAN_POINT ( 'NONE',  ( -0.6146835312500006365, -14.06466310670085562, -0.3854166673494634487 ) ) ;
#8501 = VERTEX_POINT ( 'NONE', #1934 ) ;
#8502 = EDGE_CURVE ( 'NONE', #9020, #9003, #6044, .T. ) ;
#8503 = DIRECTION ( 'NONE',  ( -1.000000000000000000, 0.000000000000000000, -0.000000000000000000 ) ) ;
#8504 = EDGE_CURVE ( 'NONE', #8384, #520, #10155, .T. ) ;
#8505 = DIRECTION ( 'NONE',  ( 0.3420201433256627732, 0.9396926207859105373, -0.000000000000000000 ) ) ;
#8506 = CARTESIAN_POINT ( 'NONE',  ( 20.12216914071655793, 6.025400000000000311, 0.000000000000000000 ) ) ;
#8507 = LINE ( 'NONE', #394, #9685 ) ;
#8508 = ORIENTED_EDGE ( 'NONE', *, *, #1118, .T. ) ;
#8509 = CARTESIAN_POINT ( 'NONE',  ( -0.7401821875142703400, 4.673326407553649808, 7.979999999999999538 ) ) ;
#8510 = LINE ( 'NONE', #7868, #9156 ) ;
#8511 = CARTESIAN_POINT ( 'NONE',  ( 4.009529358847659708, -2.042957248827953709, 6.159999999999999254 ) ) ;
#8512 = CARTESIAN_POINT ( 'NONE',  ( 0.6146835312500001924, -11.93533689329915326, -0.2604166673494633377 ) ) ;
#8513 = VERTEX_POINT ( 'NONE', #2880 ) ;
#8514 = EDGE_CURVE ( 'NONE', #2835, #6209, #1135, .T. ) ;
#8515 = ORIENTED_EDGE ( 'NONE', *, *, #7316, .F. ) ;
#8516 = DIRECTION ( 'NONE',  ( 0.000000000000000000, 0.000000000000000000, -1.000000000000000000 ) ) ;
#8517 = CARTESIAN_POINT ( 'NONE',  ( 1.999999999999975797, 15.00000000000000355, -6.000000000000009770 ) ) ;
#8518 =( REPRESENTATION_RELATIONSHIP ('NONE','NONE', #5100, #7608 ) REPRESENTATION_RELATIONSHIP_WITH_TRANSFORMATION ( #8237 )SHAPE_REPRESENTATION_RELATIONSHIP( ) );
#8519 = AXIS2_PLACEMENT_3D ( 'NONE', #7894, #2225, #2854 ) ;
#8520 = DIRECTION ( 'NONE',  ( 1.000000000000000000, 0.000000000000000000, 0.000000000000000000 ) ) ;
#8521 = ORIENTED_EDGE ( 'NONE', *, *, #7014, .T. ) ;
#8522 = CARTESIAN_POINT ( 'NONE',  ( 5.110351332421769754, 2.708615832122969191, 12.33605171672202339 ) ) ;
#8523 = CARTESIAN_POINT ( 'NONE',  ( 0.9046671180729951578, -5.711843387010016926, 9.379999999999995453 ) ) ;
#8524 = CARTESIAN_POINT ( 'NONE',  ( 2.625446233515515537, 5.152728359536502545, 11.05999999999999872 ) ) ;
#8525 = ORIENTED_EDGE ( 'NONE', *, *, #4736, .T. ) ;
#8526 = CARTESIAN_POINT ( 'NONE',  ( 0.7500000000000003331, -11.70096189432334732, -1.416666666666666741 ) ) ;
#8527 = UNCERTAINTY_MEASURE_WITH_UNIT (LENGTH_MEASURE( 1.000000000000000082E-05 ), #8220, 'distance_accuracy_value', 'NONE');
#8528 = VECTOR ( 'NONE', #9904, 1000.000000000000000 ) ;
#8529 = EDGE_LOOP ( 'NONE', ( #359, #7888, #6400, #1633, #4641 ) ) ;
#8530 = LINE ( 'NONE', #1262, #10091 ) ;
#8531 = DIRECTION ( 'NONE',  ( 0.000000000000000000, 0.000000000000000000, -1.000000000000000000 ) ) ;
#8532 = ORIENTED_EDGE ( 'NONE', *, *, #1767, .T. ) ;
#8533 = LINE ( 'NONE', #372, #3038 ) ;
#8534 = CARTESIAN_POINT ( 'NONE',  ( 18.40512053033274853, 3.750000000000000000, 0.000000000000000000 ) ) ;
#8535 = LINE ( 'NONE', #3057, #6409 ) ;
#8536 = CARTESIAN_POINT ( 'NONE',  ( 4.458484982038663169, 0.6162731882459350219, 7.683948283277975300 ) ) ;
#8537 = VERTEX_POINT ( 'NONE', #4516 ) ;
#8538 = CARTESIAN_POINT ( 'NONE',  ( 1.500000000000000222, -13.00000000000000533, -2.562500001365593416 ) ) ;
#8539 = CARTESIAN_POINT ( 'NONE',  ( -2.000000000000000000, -7.851777359434023218, 3.255701506262409506 ) ) ;
#8540 = DIRECTION ( 'NONE',  ( 1.000000000000000000, 0.000000000000000000, 0.000000000000000000 ) ) ;
#8541 = VECTOR ( 'NONE', #2379, 1000.000000000000000 ) ;
#8542 = DIRECTION ( 'NONE',  ( 1.049727191138616477E-16, -0.5150380749100571531, 0.8571673007021105573 ) ) ;
#8543 = DIRECTION ( 'NONE',  ( 1.000000000000000000, -0.000000000000000000, -0.000000000000000000 ) ) ;
#8544 = ADVANCED_FACE ( 'NONE', ( #10053 ), #4463, .T. ) ;
#8545 = CARTESIAN_POINT ( 'NONE',  ( 1.060575238724907038E-16, -11.26794919243112680, -1.937500001365593416 ) ) ;
#8546 = CARTESIAN_POINT ( 'NONE',  ( 1.272613240716556016, -10.02539999999999942, -12.00000000000000000 ) ) ;
#8547 = CARTESIAN_POINT ( 'NONE',  ( -2.148092372876330813, -4.215868657802593233, 1.259999999999999787 ) ) ;
#8548 = CARTESIAN_POINT ( 'NONE',  ( -0.6146835312500006365, -14.06466310670085562, -2.510416667349463005 ) ) ;
#8549 = COLOUR_RGB ( '', 0.72549020, 0.75294118, 0.79215686) ;
#8550 = EDGE_CURVE ( 'NONE', #3855, #10281, #1883, .T. ) ;
#8551 = CARTESIAN_POINT ( 'NONE',  ( 3.969226411068985882, -2.122056237541205981, 10.76394828327797626 ) ) ;
#8552 = DIRECTION ( 'NONE',  ( 0.3420201433256627732, 0.9396926207859105373, 0.000000000000000000 ) ) ;
#8553 = VECTOR ( 'NONE', #9972, 1000.000000000000000 ) ;
#8554 = ORIENTED_EDGE ( 'NONE', *, *, #10126, .T. ) ;
#8555 = CARTESIAN_POINT ( 'NONE',  ( 13.01080596966725622, -7.750000000000000000, 0.000000000000000000 ) ) ;
#8556 = FACE_OUTER_BOUND ( 'NONE', #9363, .T. ) ;
#8557 = DIRECTION ( 'NONE',  ( -1.000000000000000000, 0.000000000000000000, 0.000000000000000000 ) ) ;
#8558 = DIRECTION ( 'NONE',  ( -1.000000000000000000, 0.000000000000000000, -0.000000000000000000 ) ) ;
#8559 = ORIENTED_EDGE ( 'NONE', *, *, #3008, .F. ) ;
#8560 = AXIS2_PLACEMENT_3D ( 'NONE', #9155, #1685, #6704 ) ;
#8561 = DIRECTION ( 'NONE',  ( 0.3420201433256627732, 0.9396926207859105373, -0.000000000000000000 ) ) ;
#8562 =( LENGTH_UNIT ( ) NAMED_UNIT ( * ) SI_UNIT ( .MILLI., .METRE. ) );
#8563 = CARTESIAN_POINT ( 'NONE',  ( 4.009529358847659708, -2.042957248827953709, 3.359999999999999876 ) ) ;
#8564 = EDGE_CURVE ( 'NONE', #798, #8297, #9298, .T. ) ;
#8565 = CARTESIAN_POINT ( 'NONE',  ( -1.229367062500000163, -13.00000000000000533, -1.093750000682796486 ) ) ;
#8566 = ORIENTED_EDGE ( 'NONE', *, *, #7438, .T. ) ;
#8567 = AXIS2_PLACEMENT_3D ( 'NONE', #2923, #6889, #435 ) ;
#8568 = EDGE_LOOP ( 'NONE', ( #8619, #9479, #7418, #4774 ) ) ;
#8569 = CIRCLE ( 'NONE', #4001, 2.000000000000000000 ) ;
#8570 = FACE_OUTER_BOUND ( 'NONE', #9741, .T. ) ;
#8571 = DIRECTION ( 'NONE',  ( -0.9396926207859105373, -0.3420201433256627732, 0.000000000000000000 ) ) ;
#8572 = ORIENTED_EDGE ( 'NONE', *, *, #4408, .F. ) ;
#8573 = CARTESIAN_POINT ( 'NONE',  ( -2.542276634908081423, -5.195105386651227342, 7.856051716722022071 ) ) ;
#8574 = CARTESIAN_POINT ( 'NONE',  ( 27.00000000000001066, -25.00000000000000000, 0.000000000000000000 ) ) ;
#8575 = EDGE_LOOP ( 'NONE', ( #8461, #6712, #8431, #10227 ) ) ;
#8576 = EDGE_CURVE ( 'NONE', #3392, #9203, #345, .T. ) ;
#8577 = ADVANCED_FACE ( 'NONE', ( #6106 ), #9356, .T. ) ;
#8578 = CARTESIAN_POINT ( 'NONE',  ( -0.000000000000000000, -4.000000000000000000, -10.00000000000000000 ) ) ;
#8579 = VERTEX_POINT ( 'NONE', #3724 ) ;
#8580 = VERTEX_POINT ( 'NONE', #6797 ) ;
#8581 = CARTESIAN_POINT ( 'NONE',  ( -2.000000000000000000, -4.724769925181144359, -4.089810527897808079 ) ) ;
#8582 = PLANE ( 'NONE',  #4729 ) ;
#8583 = ORIENTED_EDGE ( 'NONE', *, *, #8881, .T. ) ;
#8584 = CARTESIAN_POINT ( 'NONE',  ( 0.000000000000000000, -4.000000000000000000, -12.00000000000000000 ) ) ;
#8585 = DIRECTION ( 'NONE',  ( -1.000000000000000000, -0.000000000000000000, -0.000000000000000000 ) ) ;
#8586 = CARTESIAN_POINT ( 'NONE',  ( -2.708615832122950096, -5.110351332421780413, 5.863948283277976792 ) ) ;
#8587 = EDGE_LOOP ( 'NONE', ( #9573, #6498, #3744, #10386 ) ) ;
#8588 = EDGE_CURVE ( 'NONE', #4905, #9902, #4403, .T. ) ;
#8589 = DIRECTION ( 'NONE',  ( -1.000000000000000000, -0.000000000000000000, -0.000000000000000000 ) ) ;
#8590 = CARTESIAN_POINT ( 'NONE',  ( 17.58618750323380553, -10.00000000000000000, -12.00000000000000000 ) ) ;
#8591 = PLANE ( 'NONE',  #921 ) ;
#8592 = CYLINDRICAL_SURFACE ( 'NONE', #8983, 1.500000000000000222 ) ;
#8593 = FACE_OUTER_BOUND ( 'NONE', #8474, .T. ) ;
#8594 = CYLINDRICAL_SURFACE ( 'NONE', #10271, 2.000000000000001776 ) ;
#8595 = CARTESIAN_POINT ( 'NONE',  ( 27.00000000000001066, -25.00000000000000000, 0.000000000000000000 ) ) ;
#8596 = CARTESIAN_POINT ( 'NONE',  ( 2.064922774268895811, 4.258245684917319807, 9.256051716722023315 ) ) ;
#8597 = CARTESIAN_POINT ( 'NONE',  ( 0.6146835312500001924, -11.93533689329915326, -0.1354166673494631989 ) ) ;
#8598 = CARTESIAN_POINT ( 'NONE',  ( 5.446173322633801384, 0.7727076532861675284, 4.883948283277976365 ) ) ;
#8599 = CARTESIAN_POINT ( 'NONE',  ( 0.6146835312499993043, -14.06466310670085562, 0.1979166659838698661 ) ) ;
#8600 = VERTEX_POINT ( 'NONE', #2091 ) ;
#8601 = CARTESIAN_POINT ( 'NONE',  ( 0.000000000000000000, -10.00000000000000000, -12.00000000000000000 ) ) ;
#8602 = LINE ( 'NONE', #5414, #3736 ) ;
#8603 = DIRECTION ( 'NONE',  ( 0.000000000000000000, -0.000000000000000000, 1.000000000000000000 ) ) ;
#8604 = DIRECTION ( 'NONE',  ( 0.000000000000000000, 0.000000000000000000, -1.000000000000000000 ) ) ;
#8605 = EDGE_LOOP ( 'NONE', ( #1948, #2740, #556, #92 ) ) ;
#8606 = SURFACE_STYLE_USAGE ( .BOTH. , #4571 ) ;
#8607 = CARTESIAN_POINT ( 'NONE',  ( 3.181980515339458471, 3.181980515339470461, 5.599999999999998757 ) ) ;
#8608 =( BOUNDED_CURVE ( )  B_SPLINE_CURVE ( 2, ( #20, #2347, #8973, #7972, #3249, #3349, #1716 ),
 .UNSPECIFIED., .F., .T. ) 
 B_SPLINE_CURVE_WITH_KNOTS ( ( 3, 2, 2, 3 ),
 ( 0.2500000000000000000, 0.2777777777777777901, 0.3055555555555555802, 0.3333333333333333148 ),
 .UNSPECIFIED. ) 
 CURVE ( )  GEOMETRIC_REPRESENTATION_ITEM ( )  RATIONAL_B_SPLINE_CURVE ( ( 1.000000000000000000, 0.8660254037844387076, 1.000000000000000000, 0.8660254037844387076, 1.000000000000000000, 0.8660254037844387076, 1.000000000000000000 ) ) 
 REPRESENTATION_ITEM ( '' )  );
#8609 = CARTESIAN_POINT ( 'NONE',  ( 1.229367062500000163, -13.00000000000000533, -1.843750000682796708 ) ) ;
#8610 = VERTEX_POINT ( 'NONE', #5992 ) ;
#8611 = ORIENTED_EDGE ( 'NONE', *, *, #5956, .T. ) ;
#8612 = CARTESIAN_POINT ( 'NONE',  ( -26.99999999999998934, 34.99999999999999289, 9.000000000000000000 ) ) ;
#8613 = EDGE_CURVE ( 'NONE', #8266, #8842, #2727, .T. ) ;
#8614 = CARTESIAN_POINT ( 'NONE',  ( 5.999999999999999112, -27.00000000000000711, 3.000000000000000000 ) ) ;
#8615 = ORIENTED_EDGE ( 'NONE', *, *, #3136, .T. ) ;
#8616 = CARTESIAN_POINT ( 'NONE',  ( 2.576046737280769605, -4.860232935257343456, 10.23605171672202374 ) ) ;
#8617 = CIRCLE ( 'NONE', #7774, 3.000000000000000000 ) ;
#8618 =( NAMED_UNIT ( * ) SI_UNIT ( $, .STERADIAN. ) SOLID_ANGLE_UNIT ( ) );
#8619 = ORIENTED_EDGE ( 'NONE', *, *, #6417, .T. ) ;
#8620 = CIRCLE ( 'NONE', #2535, 6.248999999999999666 ) ;
#8621 = DIRECTION ( 'NONE',  ( 0.9396926207859105373, 0.3420201433256627732, 0.000000000000000000 ) ) ;
#8622 = VERTEX_POINT ( 'NONE', #10209 ) ;
#8623 = VECTOR ( 'NONE', #10181, 1000.000000000000000 ) ;
#8624 = VERTEX_POINT ( 'NONE', #2144 ) ;
#8625 = ADVANCED_FACE ( 'NONE', ( #1083 ), #4413, .T. ) ;
#8626 = DIRECTION ( 'NONE',  ( -1.000000000000000000, -0.000000000000000000, -0.000000000000000000 ) ) ;
#8627 = AXIS2_PLACEMENT_3D ( 'NONE', #7881, #3211, #3318 ) ;
#8628 = ADVANCED_FACE ( 'NONE', ( #2938 ), #10104, .F. ) ;
#8629 = CARTESIAN_POINT ( 'NONE',  ( 0.000000000000000000, -13.00000000000000533, 2.000000000000000000 ) ) ;
#8630 = ORIENTED_EDGE ( 'NONE', *, *, #4777, .T. ) ;
#8631 = CARTESIAN_POINT ( 'NONE',  ( 8.000000000000001776, 0.000000000000000000, 0.000000000000000000 ) ) ;
#8632 = CARTESIAN_POINT ( 'NONE',  ( 1.999999999999987121, 15.00000000000000355, 5.999999999999999112 ) ) ;
#8633 = CARTESIAN_POINT ( 'NONE',  ( -2.708615832122950096, -5.110351332421780413, 8.663948283277974838 ) ) ;
#8634 = ORIENTED_EDGE ( 'NONE', *, *, #4359, .F. ) ;
#8635 = CIRCLE ( 'NONE', #8313, 1.599999999999998979 ) ;
#8636 = CARTESIAN_POINT ( 'NONE',  ( 1.500000000000000000, -13.86602540378444459, -2.104166668032260379 ) ) ;
#8637 = VECTOR ( 'NONE', #6243, 1000.000000000000000 ) ;
#8638 = DIRECTION ( 'NONE',  ( 0.000000000000000000, 0.000000000000000000, -1.000000000000000000 ) ) ;
#8639 = LINE ( 'NONE', #3809, #4806 ) ;
#8640 = ADVANCED_FACE ( 'NONE', ( #7553 ), #295, .F. ) ;
#8641 = FACE_OUTER_BOUND ( 'NONE', #5270, .T. ) ;
#8642 = AXIS2_PLACEMENT_3D ( 'NONE', #9158, #7406, #7357 ) ;
#8643 = DIRECTION ( 'NONE',  ( 0.000000000000000000, 1.807003620809173399E-15, -1.000000000000000000 ) ) ;
#8644 = LINE ( 'NONE', #1278, #10269 ) ;
#8645 = AXIS2_PLACEMENT_3D ( 'NONE', #4512, #10255, #2988 ) ;
#8646 = CARTESIAN_POINT ( 'NONE',  ( 1.500000000000000222, -13.00000000000000533, -1.000000000000000000 ) ) ;
#8647 = STYLED_ITEM ( 'NONE', ( #3999 ), #1236 ) ;
#8648 = CARTESIAN_POINT ( 'NONE',  ( 8.000000000000001776, -5.979767908488852868, 1.814490771706165351 ) ) ;
#8649 = CARTESIAN_POINT ( 'NONE',  ( 2.148092372876330369, 4.215868657802593233, 8.259999999999999787 ) ) ;
#8650 = CARTESIAN_POINT ( 'NONE',  ( 1.229367062500000163, -13.00000000000000533, -2.343750000682796486 ) ) ;
#8651 = VECTOR ( 'NONE', #9871, 1000.000000000000000 ) ;
#8652 = AXIS2_PLACEMENT_3D ( 'NONE', #3519, #6740, #2728 ) ;
#8653 = CARTESIAN_POINT ( 'NONE',  ( -2.417848759854264618, 4.940838830814694660, 12.44394828327797597 ) ) ;
#8654 = DIRECTION ( 'NONE',  ( 0.000000000000000000, -0.000000000000000000, 1.000000000000000000 ) ) ;
#8656 = ORIENTED_EDGE ( 'NONE', *, *, #1835, .T. ) ;
#8655 = AXIS2_PLACEMENT_3D ( 'NONE', #4431, #7676, #4748 ) ;
#8657 = DIRECTION ( 'NONE',  ( 0.000000000000000000, 0.000000000000000000, -1.000000000000000000 ) ) ;
#8658 = AXIS2_PLACEMENT_3D ( 'NONE', #7499, #242, #2574 ) ;
#8659 = FACE_OUTER_BOUND ( 'NONE', #7573, .T. ) ;
#8660 = DIRECTION ( 'NONE',  ( 0.000000000000000000, -1.000000000000000000, -0.000000000000000000 ) ) ;
#8661 = DIRECTION ( 'NONE',  ( -1.000000000000000000, 0.000000000000000000, 0.000000000000000000 ) ) ;
#8662 = ORIENTED_EDGE ( 'NONE', *, *, #7190, .F. ) ;
#8663 = PLANE ( 'NONE',  #8796 ) ;
#8664 = FACE_OUTER_BOUND ( 'NONE', #5184, .T. ) ;
#8665 = CARTESIAN_POINT ( 'NONE',  ( -2.148092372876330813, -4.215868657802593233, 12.45999999999999552 ) ) ;
#8666 = CARTESIAN_POINT ( 'NONE',  ( 1.229367062499999719, -13.70977540446724063, -0.8854166673494634487 ) ) ;
#8667 = ORIENTED_EDGE ( 'NONE', *, *, #2673, .F. ) ;
#8668 = ORIENTED_EDGE ( 'NONE', *, *, #480, .F. ) ;
#8669 = DIRECTION ( 'NONE',  ( 0.000000000000000000, 0.000000000000000000, 1.000000000000000000 ) ) ;
#8670 = PRESENTATION_STYLE_ASSIGNMENT (( #6275 ) ) ;
#8671 = EDGE_CURVE ( 'NONE', #1061, #2223, #2991, .T. ) ;
#8672 = ORIENTED_EDGE ( 'NONE', *, *, #6734, .F. ) ;
#8673 = CARTESIAN_POINT ( 'NONE',  ( 2.576046737280769605, -4.860232935257343456, 13.03605171672202090 ) ) ;
#8674 = ORIENTED_EDGE ( 'NONE', *, *, #4254, .F. ) ;
#8675 = CARTESIAN_POINT ( 'NONE',  ( -1.499999999999996669, -12.13397459621556607, -1.291666666666667185 ) ) ;
#8676 = CARTESIAN_POINT ( 'NONE',  ( -4.155232146225753098, 4.023224611898306158, 14.29605171672202424 ) ) ;
#8677 = PRODUCT ( 'BR-002', 'BR-002', '', ( #4039 ) ) ;
#8678 = EDGE_CURVE ( 'NONE', #6255, #8785, #1514, .T. ) ;
#8679 = EDGE_LOOP ( 'NONE', ( #6386, #2324 ) ) ;
#8680 = ORIENTED_EDGE ( 'NONE', *, *, #2477, .T. ) ;
#8681 = PLANE ( 'NONE',  #4314 ) ;
#8682 = CARTESIAN_POINT ( 'NONE',  ( 1.300000000000000044, -0.7390083445627200209, 1.280000000000001137 ) ) ;
#8683 = VERTEX_POINT ( 'NONE', #6208 ) ;
#8684 = CARTESIAN_POINT ( 'NONE',  ( 16.15239861966725599, -7.750000000000000000, -12.00000000000000000 ) ) ;
#8685 = CARTESIAN_POINT ( 'NONE',  ( 3.586028019667255595, -7.750000000000000000, -12.00000000000000000 ) ) ;
#8686 = CARTESIAN_POINT ( 'NONE',  ( 2.417848759854264618, -4.940838830814695548, 2.643948283277976596 ) ) ;
#8687 = ORIENTED_EDGE ( 'NONE', *, *, #297, .T. ) ;
#8688 = CARTESIAN_POINT ( 'NONE',  ( 0.7500000000000003331, -11.70096189432334732, -1.979166668032260157 ) ) ;
#8689 = EDGE_CURVE ( 'NONE', #2579, #8501, #1395, .T. ) ;
#8690 = ADVANCED_FACE ( 'NONE', ( #8764 ), #5525, .F. ) ;
#8691 = LINE ( 'NONE', #10290, #2764 ) ;
#8692 = DIRECTION ( 'NONE',  ( 0.000000000000000000, 0.000000000000000000, -1.000000000000000000 ) ) ;
#8693 = CARTESIAN_POINT ( 'NONE',  ( 0.7499999999999991118, -14.29903810567666333, -0.6458333346989268975 ) ) ;
#8694 = CARTESIAN_POINT ( 'NONE',  ( 0.000000000000000000, -4.000000000000000000, 0.000000000000000000 ) ) ;
#8695 = CYLINDRICAL_SURFACE ( 'NONE', #8567, 2.000000000000000000 ) ;
#8696 = FACE_OUTER_BOUND ( 'NONE', #4288, .T. ) ;
#8697 = DIRECTION ( 'NONE',  ( 0.000000000000000000, 0.000000000000000000, -1.000000000000000000 ) ) ;
#8698 = CARTESIAN_POINT ( 'NONE',  ( 2.148092372876330369, 4.215868657802593233, 2.659999999999998366 ) ) ;
#8699 = CARTESIAN_POINT ( 'NONE',  ( -0.6146835312499998594, -11.93533689329915326, -0.05208333401612993963 ) ) ;
#8700 = EDGE_CURVE ( 'NONE', #4078, #8200, #3881, .T. ) ;
#8701 = CARTESIAN_POINT ( 'NONE',  ( -3.951860609387083834, -3.826313983664940466, 11.60394828327797434 ) ) ;
#8702 = CYLINDRICAL_SURFACE ( 'NONE', #10057, 1.500000000000000222 ) ;
#8703 = VERTEX_POINT ( 'NONE', #3775 ) ;
#8704 = PRODUCT_CONTEXT ( 'NONE', #4923, 'mechanical' ) ;
#8705 = DIRECTION ( 'NONE',  ( -1.000000000000000000, -0.000000000000000000, -0.000000000000000000 ) ) ;
#8706 = CARTESIAN_POINT ( 'NONE',  ( 23.86012795928344588, -10.02539999999999942, -12.00000000000000000 ) ) ;
#8707 = DIRECTION ( 'NONE',  ( -0.3420201433256627732, 0.9396926207859105373, 0.000000000000000000 ) ) ;
#8708 = CARTESIAN_POINT ( 'NONE',  ( 0.000000000000000000, 3.750000000000000000, 0.000000000000000000 ) ) ;
#8709 = CARTESIAN_POINT ( 'NONE',  ( 0.4444353696672553311, 3.750000000000000000, -12.00000000000000000 ) ) ;
#8710 = ORIENTED_EDGE ( 'NONE', *, *, #4084, .F. ) ;
#8711 = EDGE_CURVE ( 'NONE', #2589, #2310, #10011, .T. ) ;
#8712 = VECTOR ( 'NONE', #6524, 1000.000000000000000 ) ;
#8713 = CARTESIAN_POINT ( 'NONE',  ( -4.444597532678119300, -0.7039550926810477227, 12.87999999999999901 ) ) ;
#8714 = APPLICATION_CONTEXT ( 'automotive_design' ) ;
#8715 = CARTESIAN_POINT ( 'NONE',  ( -1.500000000000000666, -13.86602540378444459, -1.208333333333333703 ) ) ;
#8716 = ORIENTED_EDGE ( 'NONE', *, *, #1637, .F. ) ;
#8717 = VERTEX_POINT ( 'NONE', #3040 ) ;
#8718 = CARTESIAN_POINT ( 'NONE',  ( 10.71950000000001424, 0.000000000000000000, 0.000000000000000000 ) ) ;
#8719 = CIRCLE ( 'NONE', #7024, 1.249999999999997558 ) ;
#8720 = CARTESIAN_POINT ( 'NONE',  ( 1.500000000000000222, -13.00000000000000533, -2.562500001365593416 ) ) ;
#8721 = ORIENTED_EDGE ( 'NONE', *, *, #7115, .F. ) ;
#8722 = CARTESIAN_POINT ( 'NONE',  ( 2.576046737280769605, -4.860232935257343456, 7.436051716722023031 ) ) ;
#8723 = CARTESIAN_POINT ( 'NONE',  ( 1.364683531250000303, -13.00000000000000533, 0.3593749989758050489 ) ) ;
#8724 =( NAMED_UNIT ( * ) PLANE_ANGLE_UNIT ( ) SI_UNIT ( $, .RADIAN. ) );
#8725 = ORIENTED_EDGE ( 'NONE', *, *, #4965, .T. ) ;
#8726 = EDGE_CURVE ( 'NONE', #935, #4422, #8822, .T. ) ;
#8727 = DIRECTION ( 'NONE',  ( 0.000000000000000000, 0.000000000000000000, -1.000000000000000000 ) ) ;
#8728 = CARTESIAN_POINT ( 'NONE',  ( 2.542276634908080535, 5.195105386651229118, 14.85605171672202296 ) ) ;
#8729 = TOROIDAL_SURFACE ( 'NONE', #5506, 2.600000000000000089, 0.1499999999999999944 ) ;
#8730 = VERTEX_POINT ( 'NONE', #9682 ) ;
#8731 = EDGE_CURVE ( 'NONE', #6440, #1730, #4566, .T. ) ;
#8732 = VECTOR ( 'NONE', #6941, 1000.000000000000000 ) ;
#8733 = ORIENTED_EDGE ( 'NONE', *, *, #9021, .F. ) ;
#8734 = DIRECTION ( 'NONE',  ( 0.9396926207859105373, 0.3420201433256627732, 0.000000000000000000 ) ) ;
#8735 = PLANE ( 'NONE',  #7449 ) ;
#8736 = ORIENTED_EDGE ( 'NONE', *, *, #6395, .T. ) ;
#8737 = DIRECTION ( 'NONE',  ( 0.000000000000000000, 0.000000000000000000, 1.000000000000000000 ) ) ;
#8738 = EDGE_CURVE ( 'NONE', #614, #3582, #2193, .T. ) ;
#8739 = DIRECTION ( 'NONE',  ( 0.000000000000000000, 0.000000000000000000, 1.000000000000000000 ) ) ;
#8740 = CARTESIAN_POINT ( 'NONE',  ( 3.951860609387084722, 3.826313983664940022, 1.803948283277976516 ) ) ;
#8741 = VERTEX_POINT ( 'NONE', #4675 ) ;
#8742 = VECTOR ( 'NONE', #221, 1000.000000000000000 ) ;
#8743 = CARTESIAN_POINT ( 'NONE',  ( -1.229367062500000163, -13.00000000000000533, -2.468750000682796486 ) ) ;
#8744 = CARTESIAN_POINT ( 'NONE',  ( -2.000000000000012879, 15.00000000000000355, 3.999999999999986233 ) ) ;
#8745 = FILL_AREA_STYLE_COLOUR ( '', #5142 ) ;
#8746 = ORIENTED_EDGE ( 'NONE', *, *, #398, .F. ) ;
#8747 = DIRECTION ( 'NONE',  ( 0.000000000000000000, 1.000000000000000000, -7.228014483236698281E-18 ) ) ;
#8748 = CARTESIAN_POINT ( 'NONE',  ( -1.500000000000000222, -13.00000000000000533, -2.312500001365593860 ) ) ;
#8749 = CARTESIAN_POINT ( 'NONE',  ( -0.7500000000000007772, -14.29903810567666156, -2.166666666666666519 ) ) ;
#8750 = FACE_OUTER_BOUND ( 'NONE', #5533, .T. ) ;
#8751 = LINE ( 'NONE', #62, #2525 ) ;
#8752 = CARTESIAN_POINT ( 'NONE',  ( -3.181980515339458027, -3.181980515339470905, 4.200000000000000178 ) ) ;
#8753 = CARTESIAN_POINT ( 'NONE',  ( 1.229367062500000163, -13.00000000000000533, -1.343750000682796486 ) ) ;
#8754 = CARTESIAN_POINT ( 'NONE',  ( 5.152728359536493663, 2.625446233515533745, 0.1399999999999999856 ) ) ;
#8755 = DIRECTION ( 'NONE',  ( -0.000000000000000000, -0.000000000000000000, 1.000000000000000000 ) ) ;
#8756 = ORIENTED_EDGE ( 'NONE', *, *, #6140, .T. ) ;
#8757 = PRODUCT_CONTEXT ( 'NONE', #4179, 'mechanical' ) ;
#8758 = CARTESIAN_POINT ( 'NONE',  ( 3.889087296526005488, 3.889087296526018811, -3.866961113726609188E-17 ) ) ;
#8759 = FACE_OUTER_BOUND ( 'NONE', #7441, .T. ) ;
#8760 = EDGE_CURVE ( 'NONE', #10319, #9335, #710, .T. ) ;
#8761 = ORIENTED_EDGE ( 'NONE', *, *, #8550, .T. ) ;
#8762 = FACE_OUTER_BOUND ( 'NONE', #9873, .T. ) ;
#8763 = EDGE_CURVE ( 'NONE', #5526, #4582, #1563, .T. ) ;
#8764 = FACE_OUTER_BOUND ( 'NONE', #2576, .T. ) ;
#8765 = PRODUCT_DEFINITION_SHAPE ( 'NONE', 'NONE',  #8792 ) ;
#8766 = VERTEX_POINT ( 'NONE', #10423 ) ;
#8767 = CARTESIAN_POINT ( 'NONE',  ( -1.500000000000000666, -13.86602540378444637, -0.2708333346989268420 ) ) ;
#8768 = DIRECTION ( 'NONE',  ( 0.000000000000000000, 1.000000000000000000, 0.000000000000000000 ) ) ;
#8769 = CARTESIAN_POINT ( 'NONE',  ( -0.7039550926810301812, -4.444597532678121965, 12.31999999999999851 ) ) ;
#8770 = CARTESIAN_POINT ( 'NONE',  ( -1.500000000000000222, -13.00000000000000533, -0.7500000000000002220 ) ) ;
#8771 = ORIENTED_EDGE ( 'NONE', *, *, #10472, .T. ) ;
#8772 = ORIENTED_EDGE ( 'NONE', *, *, #1971, .F. ) ;
#8773 = ADVANCED_FACE ( 'NONE', ( #7919 ), #7166, .F. ) ;
#8774 = CARTESIAN_POINT ( 'NONE',  ( 5.019816903233805583, -10.00000000000000000, -12.00000000000000000 ) ) ;
#8775 = CARTESIAN_POINT ( 'NONE',  ( 1.300000000000000044, 1.478016689125442484, -1.626303258728256651E-15 ) ) ;
#8776 = EDGE_LOOP ( 'NONE', ( #5692, #133, #1053, #1049 ) ) ;
#8777 = CARTESIAN_POINT ( 'NONE',  ( 2.542276634908080535, 5.195105386651229118, 14.85605171672202296 ) ) ;
#8778 = DIRECTION ( 'NONE',  ( -1.000000000000000000, -0.000000000000000000, 0.000000000000000000 ) ) ;
#8779 =( LENGTH_UNIT ( ) NAMED_UNIT ( * ) SI_UNIT ( .MILLI., .METRE. ) );
#8780 = ORIENTED_EDGE ( 'NONE', *, *, #2801, .T. ) ;
#8781 = CARTESIAN_POINT ( 'NONE',  ( 10.00000000000000000, 52.93638525830372998, 8.843061888689529582 ) ) ;
#8782 = CARTESIAN_POINT ( 'NONE',  ( 2.576046737280769605, -4.860232935257343456, 13.03605171672202090 ) ) ;
#8783 = ORIENTED_EDGE ( 'NONE', *, *, #4911, .F. ) ;
#8784 =( NAMED_UNIT ( * ) PLANE_ANGLE_UNIT ( ) SI_UNIT ( $, .RADIAN. ) );
#8785 = VERTEX_POINT ( 'NONE', #6421 ) ;
#8786 = LINE ( 'NONE', #3217, #5500 ) ;
#8787 = AXIS2_PLACEMENT_3D ( 'NONE', #5590, #3653, #10322 ) ;
#8788 = CARTESIAN_POINT ( 'NONE',  ( 0.000000000000000000, -0.7390083445627200209, 1.280000000000001137 ) ) ;
#8789 = EDGE_LOOP ( 'NONE', ( #6963, #5734, #10371, #720 ) ) ;
#8790 = CARTESIAN_POINT ( 'NONE',  ( 10.00000000000000000, -7.673322273190750664, 3.656518192455050276 ) ) ;
#8791 = DIRECTION ( 'NONE',  ( -0.7043149233066460235, 0.7043149233066439141, -0.08877487040322810941 ) ) ;
#8792 = PRODUCT_DEFINITION ( 'UNKNOWN', '', #2290, #10487 ) ;
#8793 = CARTESIAN_POINT ( 'NONE',  ( -3.951860609387083834, -3.826313983664940466, 0.4039482832779765498 ) ) ;
#8794 = ORIENTED_EDGE ( 'NONE', *, *, #10301, .F. ) ;
#8795 = CARTESIAN_POINT ( 'NONE',  ( 0.6146835312499993043, -14.06466310670085562, -2.302083334016129967 ) ) ;
#8796 = AXIS2_PLACEMENT_3D ( 'NONE', #9574, #9522, #7820 ) ;
#8797 = DIRECTION ( 'NONE',  ( 0.000000000000000000, 0.000000000000000000, -1.000000000000000000 ) ) ;
#8798 = PLANE ( 'NONE',  #3959 ) ;
#8799 = VECTOR ( 'NONE', #8737, 1000.000000000000000 ) ;
#8800 = ORIENTED_EDGE ( 'NONE', *, *, #10327, .F. ) ;
#8801 = DIRECTION ( 'NONE',  ( -1.000000000000000000, -0.000000000000000000, -0.000000000000000000 ) ) ;
#8802 = DIRECTION ( 'NONE',  ( -0.9396926207859105373, -0.3420201433256627732, 0.000000000000000000 ) ) ;
#8803 = CARTESIAN_POINT ( 'NONE',  ( 23.25451694676619496, 6.000000000000000000, -12.00000000000000000 ) ) ;
#8804 = CARTESIAN_POINT ( 'NONE',  ( 0.7499999999999991118, -14.29903810567666333, -1.083333333333333481 ) ) ;
#8805 = AXIS2_PLACEMENT_3D ( 'NONE', #1531, #1473, #9542 ) ;
#8806 = CARTESIAN_POINT ( 'NONE',  ( 11.00000000000000355, 0.000000000000000000, 0.000000000000000000 ) ) ;
#8807 = CARTESIAN_POINT ( 'NONE',  ( 4.215868657802586128, 2.148092372876346801, 11.33999999999999808 ) ) ;
#8808 = CIRCLE ( 'NONE', #4392, 6.248999999999999666 ) ;
#8809 = CARTESIAN_POINT ( 'NONE',  ( 1.229367062500000163, -13.00000000000000533, 0.1562499993172034307 ) ) ;
#8810 = CARTESIAN_POINT ( 'NONE',  ( -5.446173322633801384, -0.7727076532861678615, 6.283948283277974944 ) ) ;
#8811 = DIRECTION ( 'NONE',  ( -0.9396926207859105373, -0.3420201433256627732, 0.000000000000000000 ) ) ;
#8812 = AXIS2_PLACEMENT_3D ( 'NONE', #9310, #5328, #1201 ) ;
#8813 = EDGE_CURVE ( 'NONE', #6819, #5116, #7112, .T. ) ;
#8814 = ORIENTED_EDGE ( 'NONE', *, *, #5631, .T. ) ;
#8815 = APPLICATION_PROTOCOL_DEFINITION ( 'draft international standard', 'automotive_design', 1998, #3097 ) ;
#8816 = VECTOR ( 'NONE', #3035, 1000.000000000000000 ) ;
#8817 = CARTESIAN_POINT ( 'NONE',  ( -2.496947748567517333, 4.900535883036019058, 2.239999999999999769 ) ) ;
#8818 = AXIS2_PLACEMENT_3D ( 'NONE', #6719, #377, #3602 ) ;
#8819 = DIRECTION ( 'NONE',  ( -1.000000000000000000, -0.000000000000000000, -0.000000000000000000 ) ) ;
#8820 = ORIENTED_EDGE ( 'NONE', *, *, #227, .F. ) ;
#8821 = DIRECTION ( 'NONE',  ( 1.000000000000000000, 4.625929269271485914E-16, 0.000000000000000000 ) ) ;
#8822 = LINE ( 'NONE', #9520, #7298 ) ;
#8823 = VECTOR ( 'NONE', #8013, 1000.000000000000000 ) ;
#8824 = FACE_OUTER_BOUND ( 'NONE', #3108, .T. ) ;
#8825 = CARTESIAN_POINT ( 'NONE',  ( 3.969226411068985882, -2.122056237541205981, -0.4360517167220233636 ) ) ;
#8826 = VECTOR ( 'NONE', #9518, 1000.000000000000000 ) ;
#8827 = ADVANCED_FACE ( 'NONE', ( #6312 ), #3145, .T. ) ;
#8828 = CARTESIAN_POINT ( 'NONE',  ( 1.500000000000000444, -12.13397459621556607, -1.958333333333333481 ) ) ;
#8829 = EDGE_CURVE ( 'NONE', #6050, #9585, #6443, .T. ) ;
#8830 = ORIENTED_EDGE ( 'NONE', *, *, #233, .F. ) ;
#8831 = AXIS2_PLACEMENT_3D ( 'NONE', #494, #2143, #5941 ) ;
#8832 = ORIENTED_EDGE ( 'NONE', *, *, #1348, .T. ) ;
#8833 = CARTESIAN_POINT ( 'NONE',  ( 0.000000000000000000, 0.7390083445627193548, -1.280000000000000693 ) ) ;
#8834 = CARTESIAN_POINT ( 'NONE',  ( 1.500000000000000222, -13.00000000000000533, -2.000000000000000000 ) ) ;
#8835 = ORIENTED_EDGE ( 'NONE', *, *, #2258, .F. ) ;
#8836 = CARTESIAN_POINT ( 'NONE',  ( 1.500000000000000222, -13.00000000000000533, -3.000000000000000000 ) ) ;
#8837 = SURFACE_STYLE_USAGE ( .BOTH. , #4162 ) ;
#8838 = ORIENTED_EDGE ( 'NONE', *, *, #6252, .F. ) ;
#8839 = CARTESIAN_POINT ( 'NONE',  ( 23.25451694676619496, -10.00000000000000000, 0.000000000000000000 ) ) ;
#8840 = CARTESIAN_POINT ( 'NONE',  ( 2.122056237541221524, -3.969226411068978777, 1.836051716722023386 ) ) ;
#8841 = ADVANCED_FACE ( 'NONE', ( #1337 ), #7330, .F. ) ;
#8842 = VERTEX_POINT ( 'NONE', #2565 ) ;
#8843 = ORIENTED_EDGE ( 'NONE', *, *, #610, .T. ) ;
#8844 = CARTESIAN_POINT ( 'NONE',  ( 25.00000000000000000, -4.000000000000000000, -12.00000000000000000 ) ) ;
#8845 = EDGE_CURVE ( 'NONE', #6101, #9404, #2755, .T. ) ;
#8846 = DIRECTION ( 'NONE',  ( 0.000000000000000000, 1.000000000000000000, -1.320393690296331133E-15 ) ) ;
#8847 = EDGE_LOOP ( 'NONE', ( #6079, #7363, #9105, #6606 ) ) ;
#8848 = CARTESIAN_POINT ( 'NONE',  ( 0.8603895577212593571, 5.432285873273261068, 8.119999999999999218 ) ) ;
#8849 = DIRECTION ( 'NONE',  ( 0.000000000000000000, 1.000000000000000000, 0.000000000000000000 ) ) ;
#8850 = CARTESIAN_POINT ( 'NONE',  ( 5.711843387010018702, -0.9046671180729751738, 0.4199999999999999289 ) ) ;
#8851 = ORIENTED_EDGE ( 'NONE', *, *, #2477, .F. ) ;
#8852 = CARTESIAN_POINT ( 'NONE',  ( -1.500000000000000222, -13.00000000000000533, -0.8125000013655935271 ) ) ;
#8853 = EDGE_LOOP ( 'NONE', ( #2676, #9894, #2747, #6958 ) ) ;
#8854 = DIRECTION ( 'NONE',  ( 1.000000000000000000, 0.000000000000000000, 0.000000000000000000 ) ) ;
#8855 = DIRECTION ( 'NONE',  ( 0.000000000000000000, -0.000000000000000000, 1.000000000000000000 ) ) ;
#8856 = CARTESIAN_POINT ( 'NONE',  ( 10.00000000000000000, -6.700937042937042065, -2.183447440113260196 ) ) ;
#8857 = LINE ( 'NONE', #114, #4168 ) ;
#8858 = APPLICATION_CONTEXT ( 'automotive_design' ) ;
#8859 = AXIS2_PLACEMENT_3D ( 'NONE', #8340, #10040, #5975 ) ;
#8860 = DIRECTION ( 'NONE',  ( -1.000000000000000000, 0.000000000000000000, 0.000000000000000000 ) ) ;
#8861 = CARTESIAN_POINT ( 'NONE',  ( 4.444597532678119300, 0.7039550926810472786, 5.879999999999999893 ) ) ;
#8862 = ORIENTED_EDGE ( 'NONE', *, *, #9552, .T. ) ;
#8863 = ADVANCED_FACE ( 'NONE', ( #9781 ), #870, .F. ) ;
#8864 = CARTESIAN_POINT ( 'NONE',  ( -1.229367062500000163, -13.00000000000000533, -1.093750000682796486 ) ) ;
#8865 = CARTESIAN_POINT ( 'NONE',  ( -3.889087296526005044, -3.889087296526019255, 6.999999999999999112 ) ) ;
#8866 = DIRECTION ( 'NONE',  ( 0.000000000000000000, 1.000000000000000000, 0.000000000000000000 ) ) ;
#8867 = AXIS2_PLACEMENT_3D ( 'NONE', #923, #9994, #5785 ) ;
#8868 = APPLICATION_PROTOCOL_DEFINITION ( 'draft international standard', 'automotive_design', 1998, #4923 ) ;
#8869 = EDGE_CURVE ( 'NONE', #3855, #8167, #24, .T. ) ;
#8870 = CARTESIAN_POINT ( 'NONE',  ( 0.000000000000000000, 1.478016689125442484, -1.626303258728256651E-15 ) ) ;
#8871 = DIRECTION ( 'NONE',  ( 1.000000000000000000, 0.000000000000000000, 0.000000000000000000 ) ) ;
#8872 = FACE_OUTER_BOUND ( 'NONE', #3585, .T. ) ;
#8873 = DIRECTION ( 'NONE',  ( 0.3420201433256627732, 0.9396926207859105373, 0.000000000000000000 ) ) ;
#8874 = EDGE_CURVE ( 'NONE', #3324, #9213, #1662, .T. ) ;
#8875 = LINE ( 'NONE', #1615, #2052 ) ;
#8876 = CARTESIAN_POINT ( 'NONE',  ( 19.29399126966725575, 3.750000000000000000, -12.00000000000000000 ) ) ;
#8877 = VECTOR ( 'NONE', #4192, 1000.000000000000000 ) ;
#8878 = CARTESIAN_POINT ( 'NONE',  ( -4.458484982038663169, -0.6162731882459353550, 0.6839482832779766319 ) ) ;
#8879 = CARTESIAN_POINT ( 'NONE',  ( -0.7499999999999997780, -11.70096189432334555, -1.333333333333333481 ) ) ;
#8880 = ORIENTED_EDGE ( 'NONE', *, *, #2682, .T. ) ;
#8881 = EDGE_CURVE ( 'NONE', #9529, #1211, #5428, .T. ) ;
#8882 = VERTEX_POINT ( 'NONE', #8976 ) ;
#8883 = DIRECTION ( 'NONE',  ( -1.000000000000000000, 0.000000000000000000, 0.000000000000000000 ) ) ;
#8884 = DIRECTION ( 'NONE',  ( 0.000000000000000000, 1.000000000000000000, 0.000000000000000000 ) ) ;
#8885 = ORIENTED_EDGE ( 'NONE', *, *, #552, .F. ) ;
#8886 = DIRECTION ( 'NONE',  ( 1.000000000000000000, 0.000000000000000000, 0.000000000000000000 ) ) ;
#8887 = EDGE_CURVE ( 'NONE', #8915, #2276, #4837, .T. ) ;
#8888 = DIRECTION ( 'NONE',  ( -1.000000000000000000, -0.000000000000000000, 0.000000000000000000 ) ) ;
#8889 = ORIENTED_EDGE ( 'NONE', *, *, #10256, .F. ) ;
#8890 = COLOUR_RGB ( '', 0.66274510, 0.83137255, 0.94901961) ;
#8891 = CARTESIAN_POINT ( 'NONE',  ( 4.430710083317573655, 0.7916369971161595354, 4.076051716722022711 ) ) ;
#8892 = VERTEX_POINT ( 'NONE', #3598 ) ;
#8893 = AXIS2_PLACEMENT_3D ( 'NONE', #10407, #8116, #2390 ) ;
#8894 = LINE ( 'NONE', #9646, #434 ) ;
#8895 =( GEOMETRIC_REPRESENTATION_CONTEXT ( 3 ) GLOBAL_UNCERTAINTY_ASSIGNED_CONTEXT ( ( #5475 ) ) GLOBAL_UNIT_ASSIGNED_CONTEXT ( ( #4421, #10418, #7859 ) ) REPRESENTATION_CONTEXT ( 'NONE', 'WORKASPACE' ) );
#8896 = ORIENTED_EDGE ( 'NONE', *, *, #6802, .F. ) ;
#8897 = ADVANCED_FACE ( 'NONE', ( #8381 ), #6824, .T. ) ;
#8898 = CARTESIAN_POINT ( 'NONE',  ( 5.152728359536493663, 2.625446233515533745, 5.739999999999997549 ) ) ;
#8899 = ADVANCED_FACE ( 'NONE', ( #3251 ), #4943, .F. ) ;
#8900 = CARTESIAN_POINT ( 'NONE',  ( 10.00000000000000000, 0.000000000000000000, 0.000000000000000000 ) ) ;
#8901 = CARTESIAN_POINT ( 'NONE',  ( 2.708615832122949652, 5.110351332421781301, 12.86394828327797768 ) ) ;
#8902 = ORIENTED_EDGE ( 'NONE', *, *, #4810, .F. ) ;
#8903 = VECTOR ( 'NONE', #786, 1000.000000000000000 ) ;
#8904 = CARTESIAN_POINT ( 'NONE',  ( 1.500000000000000222, -13.00000000000000533, -1.062500001365593416 ) ) ;
#8905 = CIRCLE ( 'NONE', #10264, 1.999999999999997780 ) ;
#8906 = ORIENTED_EDGE ( 'NONE', *, *, #5708, .F. ) ;
#8907 = CARTESIAN_POINT ( 'NONE',  ( -17.00000000000000000, 19.99999999999999645, 9.000000000000000000 ) ) ;
#8908 = PLANE ( 'NONE',  #6096 ) ;
#8909 = FACE_OUTER_BOUND ( 'NONE', #7000, .T. ) ;
#8910 = ADVANCED_FACE ( 'NONE', ( #9030 ), #1718, .F. ) ;
#8911 = DIRECTION ( 'NONE',  ( -1.000000000000000000, 0.000000000000000000, 0.000000000000000000 ) ) ;
#8912 = AXIS2_PLACEMENT_3D ( 'NONE', #3926, #10245, #1432 ) ;
#8913 = LINE ( 'NONE', #6406, #6577 ) ;
#8914 = CARTESIAN_POINT ( 'NONE',  ( -3.279728542977953687, 3.411736077305369541, 3.903948283277975939 ) ) ;
#8915 = VERTEX_POINT ( 'NONE', #5627 ) ;
#8916 = CARTESIAN_POINT ( 'NONE',  ( 1.500000000000000222, -13.00000000000000533, -1.000000000000000000 ) ) ;
#8917 = ADVANCED_BREP_SHAPE_REPRESENTATION ( '', ( #4775, #2101 ), #581 ) ;
#8918 = CARTESIAN_POINT ( 'NONE',  ( 5.152728359536493663, 2.625446233515533745, 5.739999999999997549 ) ) ;
#8919 = CARTESIAN_POINT ( 'NONE',  ( -2.000000000000000000, 0.000000000000000000, 0.000000000000000000 ) ) ;
#8920 = SHAPE_DEFINITION_REPRESENTATION ( #3179, #6499 ) ;
#8921 = CARTESIAN_POINT ( 'NONE',  ( 5.019816903233805583, 6.000000000000000000, -12.00000000000000000 ) ) ;
#8922 = CYLINDRICAL_SURFACE ( 'NONE', #1801, 3.000000000000000000 ) ;
#8923 = CARTESIAN_POINT ( 'NONE',  ( 10.69739119071655686, 6.025400000000000311, 0.000000000000000000 ) ) ;
#8924 = ORIENTED_EDGE ( 'NONE', *, *, #7841, .F. ) ;
#8925 = DIRECTION ( 'NONE',  ( -0.000000000000000000, -0.000000000000000000, -1.000000000000000000 ) ) ;
#8926 = DIRECTION ( 'NONE',  ( -5.694029147589358720E-15, 0.000000000000000000, 1.000000000000000000 ) ) ;
#8927 = CARTESIAN_POINT ( 'NONE',  ( -4.458484982038663169, -0.6162731882459353550, 3.483948283277976898 ) ) ;
#8928 = DIRECTION ( 'NONE',  ( 1.000000000000000000, 0.000000000000000000, 0.000000000000000000 ) ) ;
#8929 = EDGE_LOOP ( 'NONE', ( #204, #7629, #390, #752 ) ) ;
#8930 = VERTEX_POINT ( 'NONE', #6771 ) ;
#8931 = PLANE ( 'NONE',  #8658 ) ;
#8932 = CYLINDRICAL_SURFACE ( 'NONE', #27, 8.500000000000000000 ) ;
#8933 = ORIENTED_EDGE ( 'NONE', *, *, #6029, .F. ) ;
#8934 = DIRECTION ( 'NONE',  ( -1.000000000000000000, -0.000000000000000000, -0.000000000000000000 ) ) ;
#8935 = LINE ( 'NONE', #196, #2875 ) ;
#8936 = EDGE_LOOP ( 'NONE', ( #6504, #6464, #2066, #5360 ) ) ;
#8937 = CARTESIAN_POINT ( 'NONE',  ( -4.430710083317573655, -0.7916369971161599794, 11.07605171672202182 ) ) ;
#8938 = PRODUCT ( 'piston', 'piston', '', ( #16 ) ) ;
#8939 = VERTEX_POINT ( 'NONE', #7383 ) ;
#8940 = PRESENTATION_STYLE_ASSIGNMENT (( #3215 ) ) ;
#8941 = ADVANCED_FACE ( 'NONE', ( #8872 ), #126, .F. ) ;
#8942 = EDGE_LOOP ( 'NONE', ( #7407, #2011 ) ) ;
#8943 = CARTESIAN_POINT ( 'NONE',  ( 11.29375735928344504, 6.025400000000000311, -12.00000000000000000 ) ) ;
#8944 = FACE_OUTER_BOUND ( 'NONE', #1517, .T. ) ;
#8945 = VERTEX_POINT ( 'NONE', #1111 ) ;
#8946 = CARTESIAN_POINT ( 'NONE',  ( 2.496947748567516889, -4.900535883036019946, 3.639999999999999680 ) ) ;
#8947 = CARTESIAN_POINT ( 'NONE',  ( 0.000000000000000000, -10.00000000000000000, 0.000000000000000000 ) ) ;
#8948 = CARTESIAN_POINT ( 'NONE',  ( 4.089228379062037178, -4.089228379062022967, 0.6999999999999997335 ) ) ;
#8949 = ORIENTED_EDGE ( 'NONE', *, *, #9551, .F. ) ;
#8950 = CARTESIAN_POINT ( 'NONE',  ( 0.7500000000000003331, -11.70096189432334732, -1.479166668032260157 ) ) ;
#8951 = ADVANCED_FACE ( 'NONE', ( #319 ), #8157, .F. ) ;
#8952 = SURFACE_STYLE_FILL_AREA ( #2493 ) ;
#8953 = EDGE_CURVE ( 'NONE', #9040, #3277, #8016, .T. ) ;
#8954 = AXIS2_PLACEMENT_3D ( 'NONE', #8120, #6515, #7320 ) ;
#8955 = VERTEX_POINT ( 'NONE', #3545 ) ;
#8956 = CARTESIAN_POINT ( 'NONE',  ( 1.263368396766194612, 6.000000000000000000, 0.000000000000000000 ) ) ;
#8957 = DIRECTION ( 'NONE',  ( 0.000000000000000000, -1.000000000000000000, 0.000000000000000000 ) ) ;
#8958 = CYLINDRICAL_SURFACE ( 'NONE', #2198, 1.249999999999993339 ) ;
#8959 = DIRECTION ( 'NONE',  ( -1.000000000000000000, -0.000000000000000000, -0.000000000000000000 ) ) ;
#8960 = CARTESIAN_POINT ( 'NONE',  ( 0.000000000000000000, -19.00000000000000711, 0.000000000000000000 ) ) ;
#8961 = CARTESIAN_POINT ( 'NONE',  ( 2.148092372876330369, 4.215868657802593233, 13.85999999999999766 ) ) ;
#8962 = ORIENTED_EDGE ( 'NONE', *, *, #6432, .F. ) ;
#8963 = VECTOR ( 'NONE', #3253, 1000.000000000000000 ) ;
#8964 = CARTESIAN_POINT ( 'NONE',  ( 1.229367062499999719, -13.70977540446724063, 0.1145833326505365929 ) ) ;
#8965 = AXIS2_PLACEMENT_3D ( 'NONE', #5185, #5868, #6022 ) ;
#8966 = CARTESIAN_POINT ( 'NONE',  ( 2.625446233515515537, 5.152728359536502545, 5.459999999999997300 ) ) ;
#8967 = EDGE_CURVE ( 'NONE', #9536, #1697, #8136, .T. ) ;
#8968 = FACE_OUTER_BOUND ( 'NONE', #1511, .T. ) ;
#8969 = VECTOR ( 'NONE', #10424, 1000.000000000000000 ) ;
#8970 = ITEM_DEFINED_TRANSFORMATION ( 'NONE', 'NONE', #5493,  #2101 ) ;
#8971 = CARTESIAN_POINT ( 'NONE',  ( 0.000000000000000000, -13.00000000000000533, 0.000000000000000000 ) ) ;
#8972 = VECTOR ( 'NONE', #6298, 1000.000000000000000 ) ;
#8973 = CARTESIAN_POINT ( 'NONE',  ( -0.7500000000000007772, -14.29903810567666156, -1.729166668032260157 ) ) ;
#8974 = VECTOR ( 'NONE', #2250, 1000.000000000000227 ) ;
#8975 = CARTESIAN_POINT ( 'NONE',  ( 27.00000000000001066, -34.99999999999999289, 9.000000000000000000 ) ) ;
#8976 = CARTESIAN_POINT ( 'NONE',  ( 5.999999999999999112, -27.00000000000000711, -4.000000000000000000 ) ) ;
#8977 = CARTESIAN_POINT ( 'NONE',  ( 1.999999999999984901, 35.00000000000000000, 4.000000000000008882 ) ) ;
#8978 = CARTESIAN_POINT ( 'NONE',  ( -4.687928535947287756, 0.6479879772514611780, 2.816051716722022924 ) ) ;
#8979 = DIRECTION ( 'NONE',  ( 0.000000000000000000, -1.026972870230479989E-15, -1.000000000000000000 ) ) ;
#8980 = COLOUR_RGB ( '', 0.31764706, 0.68627451, 0.89019608) ;
#8981 = CARTESIAN_POINT ( 'NONE',  ( -4.658724279160018078, 0.8323763977770419764, 0.8239482832779764232 ) ) ;
#8982 = UNCERTAINTY_MEASURE_WITH_UNIT (LENGTH_MEASURE( 1.000000000000000082E-05 ), #1784, 'distance_accuracy_value', 'NONE');
#8983 = AXIS2_PLACEMENT_3D ( 'NONE', #4657, #7957, #6194 ) ;
#8984 = FACE_BOUND ( 'NONE', #6741, .T. ) ;
#8985 = ORIENTED_EDGE ( 'NONE', *, *, #8400, .F. ) ;
#8986 = ORIENTED_EDGE ( 'NONE', *, *, #6749, .T. ) ;
#8987 = DIRECTION ( 'NONE',  ( -1.000000000000000000, -0.000000000000000000, -0.000000000000000000 ) ) ;
#8988 = AXIS2_PLACEMENT_3D ( 'NONE', #5942, #5269, #1239 ) ;
#8989 = CARTESIAN_POINT ( 'NONE',  ( 2.399999999999999911, 2.939152317953647106E-16, 6.999999999999999112 ) ) ;
#8990 = ORIENTED_EDGE ( 'NONE', *, *, #7726, .F. ) ;
#8991 = CARTESIAN_POINT ( 'NONE',  ( 2.148092372876330369, 4.215868657802594122, 5.459999999999999076 ) ) ;
#8992 = VECTOR ( 'NONE', #9981, 1000.000000000000000 ) ;
#8993 = DIRECTION ( 'NONE',  ( 0.000000000000000000, 0.000000000000000000, 1.000000000000000000 ) ) ;
#8994 = ORIENTED_EDGE ( 'NONE', *, *, #6003, .T. ) ;
#8995 = CARTESIAN_POINT ( 'NONE',  ( 4.687928535947288644, -0.6479879772514620662, 7.016051716722022213 ) ) ;
#8996 = AXIS2_PLACEMENT_3D ( 'NONE', #4081, #8957, #4821 ) ;
#8997 = CARTESIAN_POINT ( 'NONE',  ( 1.229367062500000163, -13.00000000000000533, -2.843750000682796486 ) ) ;
#8998 = ORIENTED_EDGE ( 'NONE', *, *, #4549, .F. ) ;
#8999 = ORIENTED_EDGE ( 'NONE', *, *, #8881, .F. ) ;
#9000 = EDGE_CURVE ( 'NONE', #8167, #4491, #2275, .T. ) ;
#9001 = FACE_OUTER_BOUND ( 'NONE', #1100, .T. ) ;
#9002 = FILL_AREA_STYLE ('',( #100 ) ) ;
#9003 = VERTEX_POINT ( 'NONE', #2168 ) ;
#9004 = CARTESIAN_POINT ( 'NONE',  ( -0.9046671180729963790, 5.711843387010016926, 5.179999999999999716 ) ) ;
#9005 = CARTESIAN_POINT ( 'NONE',  ( -4.900535883036028828, 2.496947748567499126, 1.959999999999999964 ) ) ;
#9006 = CARTESIAN_POINT ( 'NONE',  ( 5.195105386651219348, 2.542276634908100075, 10.34394828327797633 ) ) ;
#9007 = EDGE_LOOP ( 'NONE', ( #2155, #1931, #4593, #2954 ) ) ;
#9008 = CARTESIAN_POINT ( 'NONE',  ( -0.6146835312500006365, -14.06466310670085562, -0.8854166673494632267 ) ) ;
#9009 = EDGE_CURVE ( 'NONE', #3093, #9761, #6323, .T. ) ;
#9010 =( NAMED_UNIT ( * ) PLANE_ANGLE_UNIT ( ) SI_UNIT ( $, .RADIAN. ) );
#9011 = ORIENTED_EDGE ( 'NONE', *, *, #6094, .F. ) ;
#9012 = DIRECTION ( 'NONE',  ( 0.000000000000000000, 0.000000000000000000, -1.000000000000000000 ) ) ;
#9013 = CARTESIAN_POINT ( 'NONE',  ( -1.500000000000000222, -13.00000000000000533, -1.812500001365593416 ) ) ;
#9014 = DIRECTION ( 'NONE',  ( -0.9396926207859105373, 0.3420201433256627732, 0.000000000000000000 ) ) ;
#9015 = ORIENTED_EDGE ( 'NONE', *, *, #6863, .T. ) ;
#9016 = CARTESIAN_POINT ( 'NONE',  ( 0.000000000000000000, 18.99999999999999289, 0.000000000000000000 ) ) ;
#9017 = CARTESIAN_POINT ( 'NONE',  ( 1.229367062500000163, -13.70977540446723886, -2.385416667349463005 ) ) ;
#9018 = CARTESIAN_POINT ( 'NONE',  ( -2.148092372876330813, -4.215868657802593233, 12.45999999999999552 ) ) ;
#9019 = EDGE_CURVE ( 'NONE', #4895, #6012, #7687, .T. ) ;
#9020 = VERTEX_POINT ( 'NONE', #3802 ) ;
#9021 = EDGE_CURVE ( 'NONE', #1697, #8579, #7838, .T. ) ;
#9022 = CARTESIAN_POINT ( 'NONE',  ( 13.01080596966725622, -7.750000000000000000, 0.000000000000000000 ) ) ;
#9023 =( BOUNDED_CURVE ( )  B_SPLINE_CURVE ( 2, ( #10090, #10241, #5349, #5195, #6031, #9283, #8492 ),
 .UNSPECIFIED., .F., .T. ) 
 B_SPLINE_CURVE_WITH_KNOTS ( ( 3, 2, 2, 3 ),
 ( 0.000000000000000000, 0.02777777777777779705, 0.05555555555555559410, 0.08333333333333339810 ),
 .UNSPECIFIED. ) 
 CURVE ( )  GEOMETRIC_REPRESENTATION_ITEM ( )  RATIONAL_B_SPLINE_CURVE ( ( 1.000000000000000000, 0.8660254037844387076, 1.000000000000000000, 0.8660254037844387076, 1.000000000000000000, 0.8660254037844383745, 1.000000000000000222 ) ) 
 REPRESENTATION_ITEM ( '' )  );
#9024 = CARTESIAN_POINT ( 'NONE',  ( 5.711843387010018702, -0.9046671180729751738, 3.219999999999999751 ) ) ;
#9025 = DIRECTION ( 'NONE',  ( -0.000000000000000000, -0.000000000000000000, 1.000000000000000000 ) ) ;
#9026 = CARTESIAN_POINT ( 'NONE',  ( 2.625446233515515093, 5.152728359536503433, 11.05999999999999872 ) ) ;
#9027 = AXIS2_PLACEMENT_3D ( 'NONE', #6396, #3222, #8739 ) ;
#9028 = CARTESIAN_POINT ( 'NONE',  ( 8.000000000000001776, -4.147285340411748678, -5.698247474649444477 ) ) ;
#9029 = CARTESIAN_POINT ( 'NONE',  ( 1.500000000000002887, -12.38667738857996348, -0.03299150346530656946 ) ) ;
#9030 = FACE_OUTER_BOUND ( 'NONE', #3673, .T. ) ;
#9031 = CYLINDRICAL_SURFACE ( 'NONE', #9306, 1.500000000000000222 ) ;
#9032 = CARTESIAN_POINT ( 'NONE',  ( 2.064922774268895811, 4.258245684917319807, 6.456051716722022604 ) ) ;
#9033 = EDGE_CURVE ( 'NONE', #9713, #7594, #4494, .T. ) ;
#9034 = SURFACE_SIDE_STYLE ('',( #77 ) ) ;
#9035 = CARTESIAN_POINT ( 'NONE',  ( -4.658724279160018078, 0.8323763977770419764, 9.223948283277977112 ) ) ;
#9036 = VECTOR ( 'NONE', #4242, 1000.000000000000000 ) ;
#9037 = DIRECTION ( 'NONE',  ( 1.000000000000000000, 0.000000000000000000, 0.000000000000000000 ) ) ;
#9038 = EDGE_LOOP ( 'NONE', ( #7736, #9964, #8261, #10162 ) ) ;
#9039 = CARTESIAN_POINT ( 'NONE',  ( -2.542276634908081423, -5.195105386651227342, 7.856051716722022071 ) ) ;
#9040 = VERTEX_POINT ( 'NONE', #2965 ) ;
#9041 = DIRECTION ( 'NONE',  ( 0.9396926207859105373, 0.3420201433256627732, 0.000000000000000000 ) ) ;
#9042 = DIRECTION ( 'NONE',  ( -0.3420201433256627732, -0.9396926207859105373, 0.000000000000000000 ) ) ;
#9043 = ORIENTED_EDGE ( 'NONE', *, *, #2803, .T. ) ;
#9044 = AXIS2_PLACEMENT_3D ( 'NONE', #6030, #5194, #5247 ) ;
#9045 = ADVANCED_FACE ( 'NONE', ( #4541 ), #10186, .F. ) ;
#9046 = CARTESIAN_POINT ( 'NONE',  ( -3.345732310141667831, 3.345732310141653620, 4.899999999999999467 ) ) ;
#9047 = FACE_OUTER_BOUND ( 'NONE', #8212, .T. ) ;
#9048 = ORIENTED_EDGE ( 'NONE', *, *, #3056, .T. ) ;
#9049 = CARTESIAN_POINT ( 'NONE',  ( -3.411736077305382420, 3.279728542977939476, 11.49605171672201998 ) ) ;
#9050 = VERTEX_POINT ( 'NONE', #6186 ) ;
#9051 = VECTOR ( 'NONE', #3123, 1000.000000000000000 ) ;
#9052 = SURFACE_STYLE_USAGE ( .BOTH. , #8051 ) ;
#9053 = ORIENTED_EDGE ( 'NONE', *, *, #2403, .F. ) ;
#9054 = CARTESIAN_POINT ( 'NONE',  ( 3.535533905932731980, 3.535533905932744414, -8.174322470544786116E-18 ) ) ;
#9055 = CARTESIAN_POINT ( 'NONE',  ( 0.000000000000000000, 26.99999999999999289, 1.249999999999988898 ) ) ;
#9056 = EDGE_LOOP ( 'NONE', ( #4926, #454 ) ) ;
#9057 = CARTESIAN_POINT ( 'NONE',  ( -5.152728359536494551, -2.625446233515535077, 4.339999999999999858 ) ) ;
#9058 = CARTESIAN_POINT ( 'NONE',  ( -5.152728359536494551, -2.625446233515535077, 7.139999999999997016 ) ) ;
#9059 = MECHANICAL_DESIGN_GEOMETRIC_PRESENTATION_REPRESENTATION (  '', ( #1776 ), #6172 ) ;
#9060 = CARTESIAN_POINT ( 'NONE',  ( 5.697241258616385196, -0.9968613283357656840, 10.62394828327797569 ) ) ;
#9061 = ORIENTED_EDGE ( 'NONE', *, *, #5898, .T. ) ;
#9062 = CARTESIAN_POINT ( 'NONE',  ( -1.229367062500000163, -12.29022459553277002, -1.010416667349463449 ) ) ;
#9063 = VECTOR ( 'NONE', #5864, 1000.000000000000000 ) ;
#9064 = APPLICATION_CONTEXT ( 'automotive_design' ) ;
#9065 = SHAPE_REPRESENTATION_RELATIONSHIP ( 'NONE' , 'NONE' ,  #6499, #8040 ) ;
#9066 = AXIS2_PLACEMENT_3D ( 'NONE', #8462, #1391, #3581 ) ;
#9067 = ORIENTED_EDGE ( 'NONE', *, *, #8054, .F. ) ;
#9068 = CARTESIAN_POINT ( 'NONE',  ( 0.000000000000000000, -4.000000000000000000, -12.00000000000000000 ) ) ;
#9069 = EDGE_CURVE ( 'NONE', #7252, #8266, #10392, .T. ) ;
#9070 = DIRECTION ( 'NONE',  ( 1.156482317317871478E-16, -1.000000000000000000, -0.000000000000000000 ) ) ;
#9071 = CARTESIAN_POINT ( 'NONE',  ( 0.7500000000000003331, -11.70096189432334732, -0.9791666680322602678 ) ) ;
#9072 = ORIENTED_EDGE ( 'NONE', *, *, #2618, .T. ) ;
#9073 = PLANE ( 'NONE',  #6411 ) ;
#9074 = CARTESIAN_POINT ( 'NONE',  ( 0.6146835312500001924, -11.93533689329915326, -1.260416667349463227 ) ) ;
#9075 = CARTESIAN_POINT ( 'NONE',  ( -4.458484982038663169, -0.6162731882459353550, 0.6839482832779766319 ) ) ;
#9076 = ORIENTED_EDGE ( 'NONE', *, *, #1943, .T. ) ;
#9077 = LINE ( 'NONE', #1917, #6614 ) ;
#9078 = CARTESIAN_POINT ( 'NONE',  ( 4.900535883036028828, -2.496947748567499126, 3.359999999999999876 ) ) ;
#9079 = CARTESIAN_POINT ( 'NONE',  ( 27.00000000000001066, 35.00000000000001421, 5.999999999999999112 ) ) ;
#9080 = AXIS2_PLACEMENT_3D ( 'NONE', #9342, #2077, #3709 ) ;
#9081 = CARTESIAN_POINT ( 'NONE',  ( -2.625446233515515537, -5.152728359536502545, 6.859999999999999432 ) ) ;
#9082 = VECTOR ( 'NONE', #9460, 1000.000000000000000 ) ;
#9083 = ADVANCED_FACE ( 'NONE', ( #5292 ), #3698, .F. ) ;
#9084 = CARTESIAN_POINT ( 'NONE',  ( 0.000000000000000000, -10.00000000000000000, -12.00000000000000000 ) ) ;
#9085 = CARTESIAN_POINT ( 'NONE',  ( 0.000000000000000000, -7.063614741696270016, 8.843061888689529582 ) ) ;
#9086 = DIRECTION ( 'NONE',  ( 0.000000000000000000, -1.000000000000000000, 0.000000000000000000 ) ) ;
#9087 = CARTESIAN_POINT ( 'NONE',  ( -3.119207202478379681, -3.244753828200550139, 2.396051716722022551 ) ) ;
#9088 = CARTESIAN_POINT ( 'NONE',  ( 0.6146835312499993043, -14.06466310670085562, -2.302083334016129967 ) ) ;
#9089 = CARTESIAN_POINT ( 'NONE',  ( -1.963858260114716980, 4.049832306626327316, 1.243948283277976463 ) ) ;
#9090 = ORIENTED_EDGE ( 'NONE', *, *, #2457, .T. ) ;
#9091 = EDGE_CURVE ( 'NONE', #837, #9494, #8357, .T. ) ;
#9092 = CARTESIAN_POINT ( 'NONE',  ( -2.542276634908081423, -5.195105386651227342, 5.056051716722023137 ) ) ;
#9093 = ADVANCED_FACE ( 'NONE', ( #10133 ), #1216, .F. ) ;
#9094 = CARTESIAN_POINT ( 'NONE',  ( -29.99999999999998934, -13.00000000000000533, -1.249999999999993339 ) ) ;
#9095 = DIRECTION ( 'NONE',  ( 0.000000000000000000, -0.000000000000000000, -1.000000000000000000 ) ) ;
#9096 = VERTEX_POINT ( 'NONE', #2068 ) ;
#9097 = LINE ( 'NONE', #5846, #1852 ) ;
#9098 = CARTESIAN_POINT ( 'NONE',  ( 23.25451694676619496, 6.000000000000000000, 0.000000000000000000 ) ) ;
#9099 = ORIENTED_EDGE ( 'NONE', *, *, #885, .T. ) ;
#9100 = CARTESIAN_POINT ( 'NONE',  ( -4.430710083317573655, -0.7916369971161599794, 5.476051716722023066 ) ) ;
#9101 = CARTESIAN_POINT ( 'NONE',  ( -0.6146835312499998594, -11.93533689329915326, -2.677083334016129967 ) ) ;
#9102 = VERTEX_POINT ( 'NONE', #8632 ) ;
#9103 = EDGE_CURVE ( 'NONE', #1697, #3049, #10081, .T. ) ;
#9104 = DIRECTION ( 'NONE',  ( 1.000000000000000000, 0.000000000000000000, 0.000000000000000000 ) ) ;
#9105 = ORIENTED_EDGE ( 'NONE', *, *, #5772, .T. ) ;
#9106 = CARTESIAN_POINT ( 'NONE',  ( 24.68830583033274806, 3.750000000000000000, -12.00000000000000000 ) ) ;
#9107 = LINE ( 'NONE', #9963, #8141 ) ;
#9108 = ORIENTED_EDGE ( 'NONE', *, *, #10280, .F. ) ;
#9109 = CARTESIAN_POINT ( 'NONE',  ( -2.496947748567517333, 4.900535883036019058, 10.63999999999999879 ) ) ;
#9110 = CARTESIAN_POINT ( 'NONE',  ( -4.089228379062038066, 4.089228379062021190, 7.699999999999998401 ) ) ;
#9111 = CARTESIAN_POINT ( 'NONE',  ( 5.152728359536493663, 2.625446233515533745, 5.739999999999997549 ) ) ;
#9112 = ORIENTED_EDGE ( 'NONE', *, *, #3902, .T. ) ;
#9113 = CARTESIAN_POINT ( 'NONE',  ( -1.229367062500000385, -13.70977540446723886, -0.9270833340161298564 ) ) ;
#9114 = ORIENTED_EDGE ( 'NONE', *, *, #7353, .F. ) ;
#9115 = CARTESIAN_POINT ( 'NONE',  ( -1.499999999999998224, -13.86602540378444637, -2.708333333333333037 ) ) ;
#9116 = CARTESIAN_POINT ( 'NONE',  ( 25.00000000000000000, -7.750000000000000000, 0.000000000000000000 ) ) ;
#9117 = CARTESIAN_POINT ( 'NONE',  ( 1.868979409283444415, -10.02539999999999942, -12.00000000000000000 ) ) ;
#9118 = EDGE_LOOP ( 'NONE', ( #6431, #9048 ) ) ;
#9119 = CARTESIAN_POINT ( 'NONE',  ( 50.00005079999999680, 0.000000000000000000, 0.000000000000000000 ) ) ;
#9120 = CARTESIAN_POINT ( 'NONE',  ( 0.6146835312499993043, -14.06466310670085562, -0.9270833340161300784 ) ) ;
#9121 = CARTESIAN_POINT ( 'NONE',  ( 3.279728542977952799, -3.411736077305369541, -0.2960517167220233503 ) ) ;
#9122 = ORIENTED_EDGE ( 'NONE', *, *, #8504, .F. ) ;
#9123 = LINE ( 'NONE', #1863, #8992 ) ;
#9124 = CARTESIAN_POINT ( 'NONE',  ( 0.1499999999999973577, 0.000000000000000000, 0.000000000000000000 ) ) ;
#9125 = DIRECTION ( 'NONE',  ( -1.000000000000000000, -0.000000000000000000, -0.000000000000000000 ) ) ;
#9126 = CARTESIAN_POINT ( 'NONE',  ( 4.900535883036028828, -2.496947748567499126, 3.359999999999999876 ) ) ;
#9127 = DIRECTION ( 'NONE',  ( -1.000000000000000000, 0.000000000000000000, 0.000000000000000000 ) ) ;
#9128 = AXIS2_PLACEMENT_3D ( 'NONE', #5561, #1602, #803 ) ;
#9129 = FACE_OUTER_BOUND ( 'NONE', #1410, .T. ) ;
#9130 = CARTESIAN_POINT ( 'NONE',  ( 4.687928535947288644, -0.6479879772514620662, 4.216051716722023279 ) ) ;
#9131 = VECTOR ( 'NONE', #666, 1000.000000000000000 ) ;
#9132 = CARTESIAN_POINT ( 'NONE',  ( 1.229367062500000163, -13.00000000000000533, -2.718750000682796486 ) ) ;
#9133 = CIRCLE ( 'NONE', #7269, 3.000000000000000000 ) ;
#9134 = EDGE_CURVE ( 'NONE', #8297, #4172, #5445, .T. ) ;
#9135 = CARTESIAN_POINT ( 'NONE',  ( -3.279728542977953687, 3.411736077305369541, 6.703948283277976650 ) ) ;
#9136 = CARTESIAN_POINT ( 'NONE',  ( 8.152164709283445276, 6.025400000000000311, -12.00000000000000000 ) ) ;
#9137 = ORIENTED_EDGE ( 'NONE', *, *, #9940, .F. ) ;
#9138 = CIRCLE ( 'NONE', #7792, 1.219500000000000028 ) ;
#9139 = CARTESIAN_POINT ( 'NONE',  ( -0.7727076532861475444, -5.446173322633804048, 2.116051716722023190 ) ) ;
#9140 = CARTESIAN_POINT ( 'NONE',  ( 0.000000000000000000, 0.000000000000000000, -4.000000000000000000 ) ) ;
#9141 = DIRECTION ( 'NONE',  ( -1.000000000000000000, 0.000000000000000000, 0.000000000000000000 ) ) ;
#9142 = EDGE_LOOP ( 'NONE', ( #2987, #5464, #1219, #3209 ) ) ;
#9143 = VECTOR ( 'NONE', #2115, 1000.000000000000000 ) ;
#9144 = CARTESIAN_POINT ( 'NONE',  ( -4.215868657802586128, -2.148092372876348133, 9.939999999999997726 ) ) ;
#9145 = FILL_AREA_STYLE ('',( #5997 ) ) ;
#9146 = EDGE_CURVE ( 'NONE', #7882, #8384, #6926, .T. ) ;
#9147 = AXIS2_PLACEMENT_3D ( 'NONE', #10311, #1243, #4467 ) ;
#9148 = ADVANCED_FACE ( 'NONE', ( #523 ), #9440, .F. ) ;
#9149 = CARTESIAN_POINT ( 'NONE',  ( -0.8323763977770610722, 4.658724279160015413, 6.176051716722023244 ) ) ;
#9150 = DIRECTION ( 'NONE',  ( -0.000000000000000000, -0.000000000000000000, 1.000000000000000000 ) ) ;
#9151 = ORIENTED_EDGE ( 'NONE', *, *, #7899, .T. ) ;
#9152 = DIRECTION ( 'NONE',  ( 1.000000000000000000, 0.000000000000000000, 0.000000000000000000 ) ) ;
#9153 = PRESENTATION_LAYER_ASSIGNMENT (  '', '', ( #4235 ) ) ;
#9154 = ORIENTED_EDGE ( 'NONE', *, *, #7841, .T. ) ;
#9155 = CARTESIAN_POINT ( 'NONE',  ( 3.099999999999998757, 1.959434878635765477E-16, 1.600000000000000311 ) ) ;
#9156 = VECTOR ( 'NONE', #10373, 1000.000000000000000 ) ;
#9157 = CIRCLE ( 'NONE', #7638, 4.000000000000000000 ) ;
#9158 = CARTESIAN_POINT ( 'NONE',  ( 22.43558391966725907, -7.750000000000000000, -12.00000000000000000 ) ) ;
#9159 = ORIENTED_EDGE ( 'NONE', *, *, #9234, .T. ) ;
#9160 = CARTESIAN_POINT ( 'NONE',  ( 5.418398423912711870, 0.9480714621563913758, 4.076051716722022711 ) ) ;
#9161 = ADVANCED_BREP_SHAPE_REPRESENTATION ( '', ( #1236, #2101 ), #1104 ) ;
#9162 = CARTESIAN_POINT ( 'NONE',  ( -3.889087296526005044, -3.889087296526019255, 4.200000000000000178 ) ) ;
#9163 = VECTOR ( 'NONE', #10317, 1000.000000000000000 ) ;
#9164 = CARTESIAN_POINT ( 'NONE',  ( 3.889087296526005488, 3.889087296526018811, 5.599999999999998757 ) ) ;
#9165 = ORIENTED_EDGE ( 'NONE', *, *, #1500, .T. ) ;
#9166 = EDGE_CURVE ( 'NONE', #7999, #1996, #5239, .T. ) ;
#9167 = AXIS2_PLACEMENT_3D ( 'NONE', #7500, #6590, #9743 ) ;
#9168 = CARTESIAN_POINT ( 'NONE',  ( -2.607672531582950546E-16, -14.41955080893447416, -1.843750000682796708 ) ) ;
#9169 = AXIS2_PLACEMENT_3D ( 'NONE', #1411, #4636, #5227 ) ;
#9170 = ORIENTED_EDGE ( 'NONE', *, *, #4047, .F. ) ;
#9171 = VECTOR ( 'NONE', #8353, 1000.000000000000000 ) ;
#9172 = DIRECTION ( 'NONE',  ( -1.000000000000000000, -0.000000000000000000, -0.000000000000000000 ) ) ;
#9173 = DIRECTION ( 'NONE',  ( -1.000000000000000000, -0.000000000000000000, -0.000000000000000000 ) ) ;
#9174 = ORIENTED_EDGE ( 'NONE', *, *, #2628, .F. ) ;
#9175 = CARTESIAN_POINT ( 'NONE',  ( 1.500000000000000222, -13.00000000000000533, -2.062500001365593416 ) ) ;
#9176 = CARTESIAN_POINT ( 'NONE',  ( -2.607672531582950546E-16, -14.41955080893447416, -0.9687500006827967081 ) ) ;
#9177 = CARTESIAN_POINT ( 'NONE',  ( 0.6479879772514793856, -4.687928535947285091, 5.583948283277975655 ) ) ;
#9178 = VERTEX_POINT ( 'NONE', #8534 ) ;
#9179 = ADVANCED_FACE ( 'NONE', ( #10235 ), #5391, .F. ) ;
#9180 = DIRECTION ( 'NONE',  ( 0.3420201433256627732, 0.9396926207859105373, 0.000000000000000000 ) ) ;
#9181 = CARTESIAN_POINT ( 'NONE',  ( 0.000000000000000000, -7.750000000000000000, 0.000000000000000000 ) ) ;
#9182 = CARTESIAN_POINT ( 'NONE',  ( 1.060575238724907038E-16, -11.26794919243112680, 0.06249999863440622305 ) ) ;
#9183 = CARTESIAN_POINT ( 'NONE',  ( -2.625446233515515537, -5.152728359536502545, 4.059999999999999609 ) ) ;
#9184 = CARTESIAN_POINT ( 'NONE',  ( 8.000000000000001776, 0.000000000000000000, 0.000000000000000000 ) ) ;
#9185 = DIRECTION ( 'NONE',  ( 0.000000000000000000, 0.000000000000000000, -1.000000000000000000 ) ) ;
#9186 = CARTESIAN_POINT ( 'NONE',  ( 10.00000000000000000, -6.106419733534973915, -3.518755179752866447 ) ) ;
#9187 = CARTESIAN_POINT ( 'NONE',  ( -2.064922774268895811, -4.258245684917318918, 10.65605171672202012 ) ) ;
#9188 = FACE_OUTER_BOUND ( 'NONE', #8351, .T. ) ;
#9189 = CARTESIAN_POINT ( 'NONE',  ( 2.417848759854264618, -4.940838830814695548, 2.643948283277976596 ) ) ;
#9190 = EDGE_CURVE ( 'NONE', #7022, #1643, #1421, .T. ) ;
#9191 = CARTESIAN_POINT ( 'NONE',  ( 1.229367062500000163, -13.00000000000000533, -0.7187500006827964860 ) ) ;
#9192 = VERTEX_POINT ( 'NONE', #4071 ) ;
#9193 = CARTESIAN_POINT ( 'NONE',  ( 2.625446233515515537, 5.152728359536502545, 13.85999999999999766 ) ) ;
#9194 = CARTESIAN_POINT ( 'NONE',  ( 30.00000000000001066, 35.00000000000001421, -6.000000000000000000 ) ) ;
#9195 = EDGE_CURVE ( 'NONE', #4800, #4582, #1534, .T. ) ;
#9196 = DIRECTION ( 'NONE',  ( 0.000000000000000000, 0.000000000000000000, 1.000000000000000000 ) ) ;
#9197 = VERTEX_POINT ( 'NONE', #7308 ) ;
#9198 = CARTESIAN_POINT ( 'NONE',  ( 3.345732310141667387, -3.345732310141654064, 11.89999999999999858 ) ) ;
#9199 = VECTOR ( 'NONE', #291, 1000.000000000000000 ) ;
#9200 = LINE ( 'NONE', #7764, #6083 ) ;
#9201 = CARTESIAN_POINT ( 'NONE',  ( -3.119207202478379681, -3.244753828200550139, 13.59605171672202140 ) ) ;
#9202 = CARTESIAN_POINT ( 'NONE',  ( -1.229367062500000163, -13.00000000000000533, -2.093750000682796930 ) ) ;
#9203 = VERTEX_POINT ( 'NONE', #9545 ) ;
#9204 = DIRECTION ( 'NONE',  ( 0.000000000000000000, 0.000000000000000000, 1.000000000000000000 ) ) ;
#9205 = ORIENTED_EDGE ( 'NONE', *, *, #6286, .T. ) ;
#9206 = VECTOR ( 'NONE', #4292, 1000.000000000000000 ) ;
#9207 = DIRECTION ( 'NONE',  ( -0.000000000000000000, 1.000000000000000000, 0.000000000000000000 ) ) ;
#9208 = DIRECTION ( 'NONE',  ( 1.000000000000000000, 0.000000000000000000, 0.000000000000000000 ) ) ;
#9209 = ORIENTED_EDGE ( 'NONE', *, *, #4450, .F. ) ;
#9210 = CARTESIAN_POINT ( 'NONE',  ( -2.625446233515515981, -5.152728359536500768, 12.45999999999999552 ) ) ;
#9211 = CARTESIAN_POINT ( 'NONE',  ( -0.8603895577212598011, -5.432285873273260179, 3.919999999999999929 ) ) ;
#9212 = CARTESIAN_POINT ( 'NONE',  ( 5.711843387010018702, -0.9046671180729751738, 8.820000000000000284 ) ) ;
#9213 = VERTEX_POINT ( 'NONE', #7944 ) ;
#9214 = CARTESIAN_POINT ( 'NONE',  ( 1.229367062499999719, -13.70977540446724063, -1.760416667349463227 ) ) ;
#9215 = STYLED_ITEM ( 'NONE', ( #1055 ), #689 ) ;
#9216 = ORIENTED_EDGE ( 'NONE', *, *, #5479, .F. ) ;
#9217 = EDGE_CURVE ( 'NONE', #1592, #1146, #10399, .T. ) ;
#9218 = CARTESIAN_POINT ( 'NONE',  ( 10.00000000000000000, -6.700937042937071375, 2.183447440113169602 ) ) ;
#9219 = EDGE_CURVE ( 'NONE', #8766, #5625, #1234, .T. ) ;
#9220 = PRESENTATION_LAYER_ASSIGNMENT (  '', '', ( #259 ) ) ;
#9221 = DIRECTION ( 'NONE',  ( -1.000000000000000000, -1.156482317317871478E-16, -5.694029147589358720E-15 ) ) ;
#9222 = ORIENTED_EDGE ( 'NONE', *, *, #5582, .F. ) ;
#9223 = DIRECTION ( 'NONE',  ( 1.000000000000000000, -0.000000000000000000, -0.000000000000000000 ) ) ;
#9224 = CARTESIAN_POINT ( 'NONE',  ( 5.999999999999999112, -27.00000000000000711, -14.00000000000000178 ) ) ;
#9225 = CARTESIAN_POINT ( 'NONE',  ( -1.229367062500000163, -12.29022459553277002, -0.1354166673494631989 ) ) ;
#9226 = CARTESIAN_POINT ( 'NONE',  ( -3.969226411068985882, 2.122056237541205537, 9.363948283277975904 ) ) ;
#9227 = ORIENTED_EDGE ( 'NONE', *, *, #3734, .T. ) ;
#9228 = TOROIDAL_SURFACE ( 'NONE', #6337, 1.600000000000000311, 0.1000000000000000056 ) ;
#9229 = LINE ( 'NONE', #5087, #10356 ) ;
#9230 = EDGE_CURVE ( 'NONE', #7067, #5890, #3279, .T. ) ;
#9231 = FACE_OUTER_BOUND ( 'NONE', #5905, .T. ) ;
#9232 = PRODUCT_DEFINITION_FORMATION_WITH_SPECIFIED_SOURCE ( 'ANY', '', #9714, .NOT_KNOWN. ) ;
#9233 = DIRECTION ( 'NONE',  ( -0.000000000000000000, -1.000000000000000000, -0.000000000000000000 ) ) ;
#9234 = EDGE_CURVE ( 'NONE', #467, #8766, #10340, .T. ) ;
#9235 = CARTESIAN_POINT ( 'NONE',  ( -0.9046671180729962680, 5.711843387010016926, 13.57999999999999652 ) ) ;
#9236 = VECTOR ( 'NONE', #1895, 1000.000000000000000 ) ;
#9237 = DIRECTION ( 'NONE',  ( -1.000000000000000000, -0.000000000000000000, -0.000000000000000000 ) ) ;
#9238 = LINE ( 'NONE', #1977, #3491 ) ;
#9239 = CARTESIAN_POINT ( 'NONE',  ( -2.000000000000000000, -7.063614741696270016, 8.843061888689529582 ) ) ;
#9240 = CARTESIAN_POINT ( 'NONE',  ( -4.687928535947287756, 0.6479879772514611780, 14.01605171672202310 ) ) ;
#9241 = CARTESIAN_POINT ( 'NONE',  ( 8.692241771943169307E-17, -11.58044919106553294, -2.093750000682796486 ) ) ;
#9242 = AXIS2_PLACEMENT_3D ( 'NONE', #5094, #1869, #5145 ) ;
#9243 = CARTESIAN_POINT ( 'NONE',  ( 5.195105386651219348, 2.542276634908100075, 1.943948283277976419 ) ) ;
#9244 = CARTESIAN_POINT ( 'NONE',  ( 1.229367062500000163, -13.70977540446723886, -0.7604166673494633377 ) ) ;
#9245 = VECTOR ( 'NONE', #4619, 1000.000000000000000 ) ;
#9246 = ORIENTED_EDGE ( 'NONE', *, *, #2027, .T. ) ;
#9247 = CARTESIAN_POINT ( 'NONE',  ( -0.9968613283357868893, 5.697241258616382531, 8.976051716722020402 ) ) ;
#9248 = LINE ( 'NONE', #5524, #9082 ) ;
#9249 = AXIS2_PLACEMENT_3D ( 'NONE', #8856, #5711, #3287 ) ;
#9250 = DIRECTION ( 'NONE',  ( -1.000000000000000000, -0.000000000000000000, -0.000000000000000000 ) ) ;
#9251 = ORIENTED_EDGE ( 'NONE', *, *, #6420, .T. ) ;
#9252 = AXIS2_PLACEMENT_3D ( 'NONE', #585, #4708, #696 ) ;
#9253 = CARTESIAN_POINT ( 'NONE',  ( -4.215868657802586128, -2.148092372876348133, 7.139999999999998792 ) ) ;
#9254 = CARTESIAN_POINT ( 'NONE',  ( -2.042957248827969252, 4.009529358847651714, 2.239999999999999769 ) ) ;
#9255 = CARTESIAN_POINT ( 'NONE',  ( 1.229367062500000385, -12.29022459553277002, -0.3020833340161301339 ) ) ;
#9256 = ORIENTED_EDGE ( 'NONE', *, *, #5376, .F. ) ;
#9257 = ORIENTED_EDGE ( 'NONE', *, *, #9802, .F. ) ;
#9258 = CARTESIAN_POINT ( 'NONE',  ( 1.499999999999996669, -13.86602540378444814, -0.5416666666666670737 ) ) ;
#9259 = APPLICATION_CONTEXT ( 'automotive_design' ) ;
#9260 = CARTESIAN_POINT ( 'NONE',  ( 1.868979409283444415, 6.025400000000000311, -12.00000000000000000 ) ) ;
#9261 = ORIENTED_EDGE ( 'NONE', *, *, #1997, .T. ) ;
#9262 = CARTESIAN_POINT ( 'NONE',  ( 0.9046671180729951578, -5.711843387010016926, 9.379999999999995453 ) ) ;
#9263 = CARTESIAN_POINT ( 'NONE',  ( 2.496947748567516889, -4.900535883036019946, 12.03999999999999915 ) ) ;
#9264 = CARTESIAN_POINT ( 'NONE',  ( -0.9046671180729963790, 5.711843387010016926, 5.179999999999999716 ) ) ;
#9265 = EDGE_LOOP ( 'NONE', ( #240, #5312, #101, #9813 ) ) ;
#9266 = CARTESIAN_POINT ( 'NONE',  ( 8.000000000000001776, -6.700937042937071375, 2.183447440113169602 ) ) ;
#9267 = UNCERTAINTY_MEASURE_WITH_UNIT (LENGTH_MEASURE( 1.000000000000000082E-05 ), #5180, 'distance_accuracy_value', 'NONE');
#9268 = EDGE_CURVE ( 'NONE', #8703, #65, #3970, .T. ) ;
#9269 = ORIENTED_EDGE ( 'NONE', *, *, #1377, .T. ) ;
#9270 = DIRECTION ( 'NONE',  ( 0.000000000000000000, 0.000000000000000000, -1.000000000000000000 ) ) ;
#9271 = DIRECTION ( 'NONE',  ( -0.000000000000000000, 1.000000000000000000, 0.000000000000000000 ) ) ;
#9272 = ORIENTED_EDGE ( 'NONE', *, *, #2278, .F. ) ;
#9273 = CARTESIAN_POINT ( 'NONE',  ( 0.000000000000000000, -27.00000000000000711, 0.000000000000000000 ) ) ;
#9274 = DIRECTION ( 'NONE',  ( -0.000000000000000000, 1.000000000000000000, 0.000000000000000000 ) ) ;
#9275 = CARTESIAN_POINT ( 'NONE',  ( -2.500000000000000000, 0.000000000000000000, 3.000000000000000000 ) ) ;
#9276 = CARTESIAN_POINT ( 'NONE',  ( -4.258245684917310925, -2.064922774268914019, 6.143948283277977040 ) ) ;
#9277 = EDGE_LOOP ( 'NONE', ( #4135, #9532, #2517, #8314 ) ) ;
#9278 = DIRECTION ( 'NONE',  ( -1.000000000000000000, -0.000000000000000000, -0.000000000000000000 ) ) ;
#9279 = EDGE_CURVE ( 'NONE', #1830, #4156, #9390, .T. ) ;
#9280 = EDGE_CURVE ( 'NONE', #8250, #5138, #3621, .T. ) ;
#9281 = CARTESIAN_POINT ( 'NONE',  ( 4.900535883036028828, -2.496947748567499126, 11.75999999999999979 ) ) ;
#9282 = CARTESIAN_POINT ( 'NONE',  ( 10.00000000000000000, -7.063614741696270016, 3.730353617970412206 ) ) ;
#9283 = CARTESIAN_POINT ( 'NONE',  ( -1.500000000000002220, -12.13397459621556962, -2.791666666666666519 ) ) ;
#9284 = CARTESIAN_POINT ( 'NONE',  ( 19.29399126966725575, 3.750000000000000000, -12.00000000000000000 ) ) ;
#9285 = CARTESIAN_POINT ( 'NONE',  ( 1.500000000000000222, -12.13397459621556784, -2.020833334698926897 ) ) ;
#9286 = CARTESIAN_POINT ( 'NONE',  ( 15.52899435786730997, -15.65209171435138735, 0.000000000000000000 ) ) ;
#9287 = CARTESIAN_POINT ( 'NONE',  ( -4.173491630687863108, -2.231261971483782691, 13.73605171672202019 ) ) ;
#9288 = ADVANCED_BREP_SHAPE_REPRESENTATION ( '', ( #4489, #2101 ), #2267 ) ;
#9289 = CARTESIAN_POINT ( 'NONE',  ( -2.607672531582950546E-16, -14.41955080893447416, -0.8437500006827965970 ) ) ;
#9290 = ADVANCED_FACE ( 'NONE', ( #2489 ), #5701, .F. ) ;
#9291 = CARTESIAN_POINT ( 'NONE',  ( 5.195105386651219348, 2.542276634908100075, -0.8560517167220232926 ) ) ;
#9292 = CARTESIAN_POINT ( 'NONE',  ( -0.6146835312499998594, -11.93533689329915326, -1.052083334016129967 ) ) ;
#9293 = ORIENTED_EDGE ( 'NONE', *, *, #9009, .T. ) ;
#9294 = LINE ( 'NONE', #10305, #10014 ) ;
#9295 = VECTOR ( 'NONE', #2809, 1000.000000000000000 ) ;
#9296 = DIRECTION ( 'NONE',  ( -0.000000000000000000, 1.000000000000000000, -0.000000000000000000 ) ) ;
#9297 = DIRECTION ( 'NONE',  ( -1.000000000000000000, -0.000000000000000000, -0.000000000000000000 ) ) ;
#9298 = LINE ( 'NONE', #448, #4920 ) ;
#9299 = EDGE_LOOP ( 'NONE', ( #10002, #8843, #9606, #890 ) ) ;
#9300 = CARTESIAN_POINT ( 'NONE',  ( -4.215868657802586128, -2.148092372876348133, 12.73999999999999844 ) ) ;
#9301 = PLANE ( 'NONE',  #1530 ) ;
#9302 = VECTOR ( 'NONE', #2196, 1000.000000000000000 ) ;
#9303 = CARTESIAN_POINT ( 'NONE',  ( 4.673326407553653361, -0.7401821875142523544, 6.019999999999999574 ) ) ;
#9304 = CARTESIAN_POINT ( 'NONE',  ( 0.6146835312500001924, -11.93533689329915326, -0.7604166673494633377 ) ) ;
#9305 = ORIENTED_EDGE ( 'NONE', *, *, #1613, .T. ) ;
#9306 = AXIS2_PLACEMENT_3D ( 'NONE', #3940, #7167, #9731 ) ;
#9307 = ORIENTED_EDGE ( 'NONE', *, *, #5870, .F. ) ;
#9308 = CARTESIAN_POINT ( 'NONE',  ( -29.99999999999998934, -35.00000000000000000, 9.000000000000000000 ) ) ;
#9309 = CARTESIAN_POINT ( 'NONE',  ( 1.364683531250000303, -13.00000000000000533, -2.640625001024195395 ) ) ;
#9310 = CARTESIAN_POINT ( 'NONE',  ( 7.054542135639013677E-15, -28.99999999999999289, 0.000000000000000000 ) ) ;
#9311 = ORIENTED_EDGE ( 'NONE', *, *, #6815, .T. ) ;
#9312 = AXIS2_PLACEMENT_3D ( 'NONE', #4416, #9901, #5162 ) ;
#9313 = CARTESIAN_POINT ( 'NONE',  ( 3.889087296526005488, 3.889087296526018811, 11.19999999999999751 ) ) ;
#9314 = CARTESIAN_POINT ( 'NONE',  ( -2.496947748567517333, 4.900535883036019058, 13.43999999999999950 ) ) ;
#9315 = EDGE_CURVE ( 'NONE', #9096, #7164, #8042, .T. ) ;
#9316 = CARTESIAN_POINT ( 'NONE',  ( 5.432285873273257515, 0.8603895577212793411, 5.879999999999999893 ) ) ;
#9317 = ORIENTED_EDGE ( 'NONE', *, *, #1658, .T. ) ;
#9318 = DIRECTION ( 'NONE',  ( -1.000000000000000000, 0.000000000000000000, -0.000000000000000000 ) ) ;
#9319 = VECTOR ( 'NONE', #7827, 1000.000000000000000 ) ;
#9320 = ADVANCED_FACE ( 'NONE', ( #1691 ), #8165, .T. ) ;
#9321 = FILL_AREA_STYLE_COLOUR ( '', #8890 ) ;
#9322 = AXIS2_PLACEMENT_3D ( 'NONE', #6210, #5473, #652 ) ;
#9323 = ORIENTED_EDGE ( 'NONE', *, *, #10242, .F. ) ;
#9324 = VECTOR ( 'NONE', #119, 1000.000000000000000 ) ;
#9325 = DIRECTION ( 'NONE',  ( -1.000000000000000000, -0.000000000000000000, -0.000000000000000000 ) ) ;
#9326 = CARTESIAN_POINT ( 'NONE',  ( 10.69739119071655686, -10.02539999999999942, -12.00000000000000000 ) ) ;
#9327 = VECTOR ( 'NONE', #5865, 1000.000000000000227 ) ;
#9328 = VERTEX_POINT ( 'NONE', #4698 ) ;
#9329 = DIRECTION ( 'NONE',  ( 0.000000000000000000, 0.000000000000000000, -1.000000000000000000 ) ) ;
#9330 = AXIS2_PLACEMENT_3D ( 'NONE', #6157, #4306, #2830 ) ;
#9331 = EDGE_CURVE ( 'NONE', #3641, #5372, #1590, .T. ) ;
#9332 = CARTESIAN_POINT ( 'NONE',  ( 1.300000000000000044, 1.478016689125442484, -1.626303258728256651E-15 ) ) ;
#9333 = DIRECTION ( 'NONE',  ( 0.000000000000000000, 0.000000000000000000, 1.000000000000000000 ) ) ;
#9334 = CARTESIAN_POINT ( 'NONE',  ( 1.963858260114715870, -4.049832306626327316, 5.443948283277975975 ) ) ;
#9335 = VERTEX_POINT ( 'NONE', #2436 ) ;
#9336 = CARTESIAN_POINT ( 'NONE',  ( -0.7500000000000007772, -14.29903810567666156, -2.229166668032259935 ) ) ;
#9337 = CIRCLE ( 'NONE', #185, 3.000000000000000000 ) ;
#9338 = CARTESIAN_POINT ( 'NONE',  ( 10.68814634676619590, 6.000000000000000000, 0.000000000000000000 ) ) ;
#9339 = CIRCLE ( 'NONE', #34, 3.000000000000000000 ) ;
#9340 = CARTESIAN_POINT ( 'NONE',  ( -29.99999999999998934, -13.00000000000000533, 0.000000000000000000 ) ) ;
#9341 = CARTESIAN_POINT ( 'NONE',  ( -1.500000000000000222, -13.00000000000000533, -0.2500000000000002220 ) ) ;
#9342 = CARTESIAN_POINT ( 'NONE',  ( 13.01080596966725622, -7.750000000000000000, -12.00000000000000000 ) ) ;
#9343 = EDGE_CURVE ( 'NONE', #8683, #145, #3462, .T. ) ;
#9344 = FACE_OUTER_BOUND ( 'NONE', #9638, .T. ) ;
#9345 = DIRECTION ( 'NONE',  ( 0.000000000000000000, 0.000000000000000000, 1.000000000000000000 ) ) ;
#9346 = CARTESIAN_POINT ( 'NONE',  ( 4.215868657802586128, 2.148092372876346801, 0.1400000000000000411 ) ) ;
#9347 = CARTESIAN_POINT ( 'NONE',  ( -0.6146835312499998594, -11.93533689329915326, -2.177083334016129967 ) ) ;
#9348 = CARTESIAN_POINT ( 'NONE',  ( -2.417848759854264618, 4.940838830814694660, 4.043948283277976508 ) ) ;
#9349 = CARTESIAN_POINT ( 'NONE',  ( -2.607672531582950546E-16, -14.41955080893447416, -0.8437500006827965970 ) ) ;
#9350 = ORIENTED_EDGE ( 'NONE', *, *, #3234, .T. ) ;
#9351 = DIRECTION ( 'NONE',  ( -1.000000000000000000, 0.000000000000000000, -0.000000000000000000 ) ) ;
#9352 = EDGE_CURVE ( 'NONE', #2796, #7411, #791, .T. ) ;
#9353 = DIRECTION ( 'NONE',  ( -1.000000000000000000, 0.000000000000000000, 0.000000000000000000 ) ) ;
#9354 = CARTESIAN_POINT ( 'NONE',  ( 9.000000000000000000, 19.99999999999999645, 15.00000000000000000 ) ) ;
#9355 = EDGE_CURVE ( 'NONE', #3874, #4442, #7250, .T. ) ;
#9356 = PLANE ( 'NONE',  #693 ) ;
#9357 = ORIENTED_EDGE ( 'NONE', *, *, #4736, .F. ) ;
#9358 = CARTESIAN_POINT ( 'NONE',  ( 3.181980515339458471, 3.181980515339470461, 13.99999999999999822 ) ) ;
#9359 = CARTESIAN_POINT ( 'NONE',  ( 1.300000000000000044, 1.478016689125442484, -1.626303258728256651E-15 ) ) ;
#9360 = CARTESIAN_POINT ( 'NONE',  ( -4.215868657802586128, -2.148092372876348133, 1.540000000000000036 ) ) ;
#9361 =( BOUNDED_CURVE ( )  B_SPLINE_CURVE ( 2, ( #5681, #2127, #2177, #5455, #3129, #7904, #1487 ),
 .UNSPECIFIED., .F., .T. ) 
 B_SPLINE_CURVE_WITH_KNOTS ( ( 3, 2, 2, 3 ),
 ( 0.1666666666666666574, 0.1944444444444444198, 0.2222222222222221544, 0.2499999999999999167 ),
 .UNSPECIFIED. ) 
 CURVE ( )  GEOMETRIC_REPRESENTATION_ITEM ( )  RATIONAL_B_SPLINE_CURVE ( ( 1.000000000000000000, 0.8660254037844387076, 1.000000000000000000, 0.8660254037844387076, 1.000000000000000000, 0.8660254037844391517, 0.9999999999999995559 ) ) 
 REPRESENTATION_ITEM ( '' )  );
#9362 = CARTESIAN_POINT ( 'NONE',  ( -1.500000000000000666, -13.86602540378444459, -2.708333333333333481 ) ) ;
#9363 = EDGE_LOOP ( 'NONE', ( #5063, #8761, #3155, #9482 ) ) ;
#9364 = ORIENTED_EDGE ( 'NONE', *, *, #2265, .F. ) ;
#9365 = EDGE_CURVE ( 'NONE', #7779, #144, #5549, .T. ) ;
#9366 = CYLINDRICAL_SURFACE ( 'NONE', #4750, 6.248999999999999666 ) ;
#9367 = VECTOR ( 'NONE', #2118, 1000.000000000000114 ) ;
#9368 = LINE ( 'NONE', #559, #6087 ) ;
#9369 = ORIENTED_EDGE ( 'NONE', *, *, #10472, .F. ) ;
#9370 = CARTESIAN_POINT ( 'NONE',  ( -4.155232146225753098, 4.023224611898306158, 11.49605171672201998 ) ) ;
#9371 = CARTESIAN_POINT ( 'NONE',  ( 4.900535883036028828, -2.496947748567499126, 8.959999999999999076 ) ) ;
#9372 = CYLINDRICAL_SURFACE ( 'NONE', #668, 2.000000000000001776 ) ;
#9373 = ORIENTED_EDGE ( 'NONE', *, *, #2027, .F. ) ;
#9374 = CARTESIAN_POINT ( 'NONE',  ( 1.060575238724907038E-16, -11.26794919243112680, -1.375000000000000222 ) ) ;
#9375 = PRODUCT_DEFINITION_CONTEXT ( 'detailed design', #54, 'design' ) ;
#9376 = EDGE_LOOP ( 'NONE', ( #7074, #7247, #4019 ) ) ;
#9377 = AXIS2_PLACEMENT_3D ( 'NONE', #5347, #1481, #6293 ) ;
#9378 = ORIENTED_EDGE ( 'NONE', *, *, #3054, .T. ) ;
#9379 = CARTESIAN_POINT ( 'NONE',  ( 0.000000000000000000, 6.000000000000000000, -12.00000000000000000 ) ) ;
#9380 = DIRECTION ( 'NONE',  ( 0.000000000000000000, 0.000000000000000000, -1.000000000000000000 ) ) ;
#9381 = ORIENTED_EDGE ( 'NONE', *, *, #2733, .T. ) ;
#9382 = DIRECTION ( 'NONE',  ( 0.000000000000000000, 0.000000000000000000, -1.000000000000000000 ) ) ;
#9383 = CARTESIAN_POINT ( 'NONE',  ( 10.00000000000000000, 7.008469740302802897, 0.7425307242148025955 ) ) ;
#9384 = CARTESIAN_POINT ( 'NONE',  ( -0.6479879772514802738, 4.687928535947285091, 9.783948283277975833 ) ) ;
#9385 = ORIENTED_EDGE ( 'NONE', *, *, #8389, .T. ) ;
#9386 = CARTESIAN_POINT ( 'NONE',  ( 8.000000000000001776, -6.200809695932771426, -0.7745709230445765314 ) ) ;
#9387 = CARTESIAN_POINT ( 'NONE',  ( -0.7499999999999997780, -11.70096189432334555, -0.3958333346989269530 ) ) ;
#9388 = DIRECTION ( 'NONE',  ( 0.000000000000000000, 2.309263891220325920E-14, -1.000000000000000000 ) ) ;
#9389 = ADVANCED_FACE ( 'NONE', ( #7197 ), #8108, .T. ) ;
#9390 = CIRCLE ( 'NONE', #8208, 8.500000000000000000 ) ;
#9391 = CARTESIAN_POINT ( 'NONE',  ( 20.12216914071655793, 6.025400000000000311, -12.00000000000000000 ) ) ;
#9392 = DIRECTION ( 'NONE',  ( -1.000000000000000000, -0.000000000000000000, -0.000000000000000000 ) ) ;
#9393 = CARTESIAN_POINT ( 'NONE',  ( 1.878224253233805818, 6.000000000000000000, 0.000000000000000000 ) ) ;
#9394 = PLANE ( 'NONE',  #3823 ) ;
#9395 = CARTESIAN_POINT ( 'NONE',  ( -2.000000000000000000, 0.000000000000000000, 0.000000000000000000 ) ) ;
#9396 = CARTESIAN_POINT ( 'NONE',  ( 4.009529358847659708, -2.042957248827953709, 0.5599999999999999423 ) ) ;
#9397 = CARTESIAN_POINT ( 'NONE',  ( 8.692241771943169307E-17, -11.58044919106553294, -2.718750000682796042 ) ) ;
#9398 =( GEOMETRIC_REPRESENTATION_CONTEXT ( 3 ) GLOBAL_UNCERTAINTY_ASSIGNED_CONTEXT ( ( #3888 ) ) GLOBAL_UNIT_ASSIGNED_CONTEXT ( ( #10391, #2111, #5543 ) ) REPRESENTATION_CONTEXT ( 'NONE', 'WORKASPACE' ) );
#9399 = AXIS2_PLACEMENT_3D ( 'NONE', #7541, #9086, #1820 ) ;
#9400 = CARTESIAN_POINT ( 'NONE',  ( 3.244753828200538148, 3.119207202478391672, 10.20394828327797399 ) ) ;
#9401 = CARTESIAN_POINT ( 'NONE',  ( 1.229367062500000163, -13.70977540446723886, -0.2604166673494633377 ) ) ;
#9402 = VECTOR ( 'NONE', #1803, 1000.000000000000000 ) ;
#9403 = ADVANCED_FACE ( 'NONE', ( #258 ), #3674, .T. ) ;
#9404 = VERTEX_POINT ( 'NONE', #9338 ) ;
#9405 = CARTESIAN_POINT ( 'NONE',  ( -3.181725716174720991E-16, -14.73205080756888563, -2.187500001365593416 ) ) ;
#9406 = AXIS2_PLACEMENT_3D ( 'NONE', #6806, #5852, #9104 ) ;
#9407 = CARTESIAN_POINT ( 'NONE',  ( 11.00000000000000355, 0.000000000000000000, 1.219500000000000028 ) ) ;
#9408 = CARTESIAN_POINT ( 'NONE',  ( 1.263368396766194612, -10.00000000000000000, 0.000000000000000000 ) ) ;
#9409 = DIRECTION ( 'NONE',  ( 0.000000000000000000, 1.000000000000000000, -7.228014483236698281E-18 ) ) ;
#9410 = ORIENTED_EDGE ( 'NONE', *, *, #2792, .T. ) ;
#9411 = AXIS2_PLACEMENT_3D ( 'NONE', #10180, #419, #7683 ) ;
#9412 = CARTESIAN_POINT ( 'NONE',  ( -1.387778780781445991E-14, 15.00000000000000355, 0.000000000000000000 ) ) ;
#9413 = LINE ( 'NONE', #2147, #1190 ) ;
#9414 = CIRCLE ( 'NONE', #783, 2.750000000000000000 ) ;
#9415 = CARTESIAN_POINT ( 'NONE',  ( -0.7039550926810301812, -4.444597532678121965, 1.119999999999999885 ) ) ;
#9416 = ADVANCED_FACE ( 'NONE', ( #6934 ), #278, .F. ) ;
#9417 = ADVANCED_FACE ( 'NONE', ( #9231 ), #1067, .F. ) ;
#9418 = CARTESIAN_POINT ( 'NONE',  ( -2.607672531582950546E-16, -14.41955080893447416, -0.4687500006827967081 ) ) ;
#9419 = EDGE_CURVE ( 'NONE', #4407, #4215, #3703, .T. ) ;
#9420 = VERTEX_POINT ( 'NONE', #7693 ) ;
#9421 = AXIS2_PLACEMENT_3D ( 'NONE', #7562, #7667, #6054 ) ;
#9422 = ORIENTED_EDGE ( 'NONE', *, *, #1778, .F. ) ;
#9423 = AXIS2_PLACEMENT_3D ( 'NONE', #6836, #10093, #7750 ) ;
#9424 = FACE_OUTER_BOUND ( 'NONE', #5022, .T. ) ;
#9425 = DIRECTION ( 'NONE',  ( -1.000000000000000000, -0.000000000000000000, -0.000000000000000000 ) ) ;
#9426 = EDGE_LOOP ( 'NONE', ( #2904, #3474, #8771, #3994 ) ) ;
#9427 = CARTESIAN_POINT ( 'NONE',  ( 3.826313983664925811, 3.951860609387098044, 9.396051716722022107 ) ) ;
#9428 = CARTESIAN_POINT ( 'NONE',  ( 0.000000000000000000, 3.750000000000000000, 0.000000000000000000 ) ) ;
#9429 = ORIENTED_EDGE ( 'NONE', *, *, #3917, .F. ) ;
#9430 = SHAPE_REPRESENTATION ( 'pin', ( #2101 ), #2267 ) ;
#9431 = CARTESIAN_POINT ( 'NONE',  ( 15.52899435786730997, 11.65209171435138735, 0.000000000000000000 ) ) ;
#9432 = EDGE_CURVE ( 'NONE', #6552, #3824, #7534, .T. ) ;
#9433 = ORIENTED_EDGE ( 'NONE', *, *, #427, .T. ) ;
#9434 =( LENGTH_UNIT ( ) NAMED_UNIT ( * ) SI_UNIT ( .MILLI., .METRE. ) );
#9435 = VERTEX_POINT ( 'NONE', #5193 ) ;
#9436 = LINE ( 'NONE', #5288, #4832 ) ;
#9437 = CARTESIAN_POINT ( 'NONE',  ( 25.57717656966725883, -7.750000000000000000, -12.00000000000000000 ) ) ;
#9438 = EDGE_LOOP ( 'NONE', ( #8800, #4180, #6774, #5635 ) ) ;
#9439 = DIRECTION ( 'NONE',  ( 1.000000000000000000, 2.312964634635742957E-16, -0.000000000000000000 ) ) ;
#9440 = CYLINDRICAL_SURFACE ( 'NONE', #730, 2.000000000000001776 ) ;
#9441 = CARTESIAN_POINT ( 'NONE',  ( 5.697241258616385196, -0.9968613283357656840, 7.823948283277974980 ) ) ;
#9442 = VERTEX_POINT ( 'NONE', #8539 ) ;
#9443 = CARTESIAN_POINT ( 'NONE',  ( 15.26352788033274699, 3.750000000000000000, -12.00000000000000000 ) ) ;
#9444 = CARTESIAN_POINT ( 'NONE',  ( 9.869213319667256457, 3.750000000000000000, -12.00000000000000000 ) ) ;
#9445 = CARTESIAN_POINT ( 'NONE',  ( 1.500000000000000222, -13.00000000000000533, -1.062500001365593416 ) ) ;
#9446 = PRODUCT_DEFINITION_SHAPE ( 'NONE', 'NONE',  #4567 ) ;
#9447 = CARTESIAN_POINT ( 'NONE',  ( -4.900535883036028828, 2.496947748567499126, 13.15999999999999837 ) ) ;
#9448 = DIRECTION ( 'NONE',  ( -1.000000000000000000, -1.156482317317871478E-16, 5.204170427930421283E-15 ) ) ;
#9449 = DIRECTION ( 'NONE',  ( 0.000000000000000000, 0.000000000000000000, -1.000000000000000000 ) ) ;
#9450 = DIRECTION ( 'NONE',  ( 0.000000000000000000, 0.000000000000000000, -1.000000000000000000 ) ) ;
#9451 = PLANE ( 'NONE',  #2182 ) ;
#9452 = CARTESIAN_POINT ( 'NONE',  ( 3.181980515339458471, 3.181980515339470461, 2.799999999999999378 ) ) ;
#9453 = EDGE_CURVE ( 'NONE', #2420, #165, #2932, .T. ) ;
#9454 = CARTESIAN_POINT ( 'NONE',  ( 1.229367062500000163, -13.00000000000000533, -0.2187500006827964583 ) ) ;
#9455 = CARTESIAN_POINT ( 'NONE',  ( 5.697241258616385196, -0.9968613283357656840, 10.62394828327797569 ) ) ;
#9456 = DIRECTION ( 'NONE',  ( 0.000000000000000000, 1.000000000000000000, 0.000000000000000000 ) ) ;
#9457 = ORIENTED_EDGE ( 'NONE', *, *, #1260, .T. ) ;
#9458 = CARTESIAN_POINT ( 'NONE',  ( 10.00000000000000000, 8.357095590591340439, -1.552080310331536372 ) ) ;
#9459 = CARTESIAN_POINT ( 'NONE',  ( 0.000000000000000000, 26.99999999999999289, 1.249999999999993339 ) ) ;
#9460 = DIRECTION ( 'NONE',  ( 0.000000000000000000, 0.000000000000000000, 1.000000000000000000 ) ) ;
#9461 = DIRECTION ( 'NONE',  ( -1.000000000000000000, -4.625929269271485914E-16, 0.000000000000000000 ) ) ;
#9462 = ORIENTED_EDGE ( 'NONE', *, *, #2498, .T. ) ;
#9463 = EDGE_CURVE ( 'NONE', #10205, #10233, #1273, .T. ) ;
#9464 = CARTESIAN_POINT ( 'NONE',  ( 1.499999999999996669, -13.86602540378444814, -0.1041666680322604899 ) ) ;
#9465 = LINE ( 'NONE', #2304, #8974 ) ;
#9466 = CARTESIAN_POINT ( 'NONE',  ( 0.7039550926810297371, 4.444597532678122853, 10.91999999999999993 ) ) ;
#9467 = CARTESIAN_POINT ( 'NONE',  ( -0.7499999999999997780, -11.70096189432334555, -2.833333333333333481 ) ) ;
#9468 = CIRCLE ( 'NONE', #4371, 8.500000000000000000 ) ;
#9469 = EDGE_LOOP ( 'NONE', ( #9968, #459, #7159, #426 ) ) ;
#9470 = ORIENTED_EDGE ( 'NONE', *, *, #7065, .F. ) ;
#9471 = DIRECTION ( 'NONE',  ( 0.000000000000000000, 0.000000000000000000, 1.000000000000000000 ) ) ;
#9472 = FACE_OUTER_BOUND ( 'NONE', #8106, .T. ) ;
#9473 = ORIENTED_EDGE ( 'NONE', *, *, #343, .T. ) ;
#9474 = ADVANCED_FACE ( 'NONE', ( #7744 ), #4445, .T. ) ;
#9475 = CARTESIAN_POINT ( 'NONE',  ( -4.155232146225753098, 4.023224611898306158, 5.896051716722023883 ) ) ;
#9476 = EDGE_CURVE ( 'NONE', #7456, #6865, #7696, .T. ) ;
#9477 =( GEOMETRIC_REPRESENTATION_CONTEXT ( 3 ) GLOBAL_UNCERTAINTY_ASSIGNED_CONTEXT ( ( #2061 ) ) GLOBAL_UNIT_ASSIGNED_CONTEXT ( ( #1397, #5528, #3094 ) ) REPRESENTATION_CONTEXT ( 'NONE', 'WORKASPACE' ) );
#9478 = DIRECTION ( 'NONE',  ( 0.000000000000000000, 0.000000000000000000, 1.000000000000000000 ) ) ;
#9479 = ORIENTED_EDGE ( 'NONE', *, *, #984, .T. ) ;
#9480 = DIRECTION ( 'NONE',  ( 0.3420201433256627732, -0.9396926207859105373, 0.000000000000000000 ) ) ;
#9481 = VECTOR ( 'NONE', #2616, 1000.000000000000000 ) ;
#9482 = ORIENTED_EDGE ( 'NONE', *, *, #9000, .F. ) ;
#9483 =( NAMED_UNIT ( * ) SI_UNIT ( $, .STERADIAN. ) SOLID_ANGLE_UNIT ( ) );
#9484 = AXIS2_PLACEMENT_3D ( 'NONE', #5766, #8172, #7417 ) ;
#9485 = ORIENTED_EDGE ( 'NONE', *, *, #8887, .F. ) ;
#9486 = CARTESIAN_POINT ( 'NONE',  ( 1.300000000000000044, 0.7390083445627193548, -1.280000000000000693 ) ) ;
#9487 = CIRCLE ( 'NONE', #8627, 3.000000000000000000 ) ;
#9488 = CARTESIAN_POINT ( 'NONE',  ( 27.00000000000001066, -34.99999999999999289, -6.000000000000000000 ) ) ;
#9489 = EDGE_LOOP ( 'NONE', ( #7767, #3041, #5325, #4473 ) ) ;
#9490 = EDGE_CURVE ( 'NONE', #4979, #931, #7040, .T. ) ;
#9491 = PLANE ( 'NONE',  #3713 ) ;
#9492 = DIRECTION ( 'NONE',  ( -0.000000000000000000, -0.000000000000000000, 1.000000000000000000 ) ) ;
#9493 = CARTESIAN_POINT ( 'NONE',  ( 3.951860609387084722, 3.826313983664940022, 7.403948283277976827 ) ) ;
#9494 = VERTEX_POINT ( 'NONE', #7793 ) ;
#9495 = AXIS2_PLACEMENT_3D ( 'NONE', #9862, #8162, #1793 ) ;
#9496 = CARTESIAN_POINT ( 'NONE',  ( -0.7499999999999997780, -11.70096189432334555, -2.395833334698926897 ) ) ;
#9497 = VECTOR ( 'NONE', #7170, 1000.000000000000000 ) ;
#9498 = DIRECTION ( 'NONE',  ( -0.7071067811865335839, 8.659560562355102956E-17, -0.7071067811865614505 ) ) ;
#9499 = LINE ( 'NONE', #1428, #10409 ) ;
#9500 = CYLINDRICAL_SURFACE ( 'NONE', #8893, 4.000000000000000000 ) ;
#9501 = CIRCLE ( 'NONE', #3905, 2.500000000000000000 ) ;
#9502 = DIRECTION ( 'NONE',  ( 0.000000000000000000, 0.000000000000000000, 1.000000000000000000 ) ) ;
#9503 = DIRECTION ( 'NONE',  ( 0.000000000000000000, 0.000000000000000000, 1.000000000000000000 ) ) ;
#9504 = EDGE_CURVE ( 'NONE', #8537, #3139, #10404, .T. ) ;
#9505 = CARTESIAN_POINT ( 'NONE',  ( 0.000000000000000000, 0.7390083445627193548, -1.280000000000000693 ) ) ;
#9506 = AXIS2_PLACEMENT_3D ( 'NONE', #4840, #8925, #6533 ) ;
#9507 = DIRECTION ( 'NONE',  ( 1.000000000000000000, 0.000000000000000000, 0.000000000000000000 ) ) ;
#9508 = CARTESIAN_POINT ( 'NONE',  ( 0.7039550926810297371, 4.444597532678122853, 10.91999999999999993 ) ) ;
#9509 = CARTESIAN_POINT ( 'NONE',  ( -1.229367062500000385, -13.70977540446723886, 0.07291666598387017140 ) ) ;
#9510 = VECTOR ( 'NONE', #5779, 1000.000000000000000 ) ;
#9511 = CARTESIAN_POINT ( 'NONE',  ( 3.951860609387084722, 3.826313983664940022, 10.20394828327797399 ) ) ;
#9512 = FACE_BOUND ( 'NONE', #5706, .T. ) ;
#9513 = ORIENTED_EDGE ( 'NONE', *, *, #10459, .F. ) ;
#9514 = APPLICATION_PROTOCOL_DEFINITION ( 'draft international standard', 'automotive_design', 1998, #6884 ) ;
#9515 = CARTESIAN_POINT ( 'NONE',  ( 0.7499999999999991118, -14.29903810567666333, -2.145833334698926897 ) ) ;
#9516 = EDGE_CURVE ( 'NONE', #9197, #409, #2280, .T. ) ;
#9517 = CARTESIAN_POINT ( 'NONE',  ( 1.999999999999973577, 35.00000000000000000, -6.000000000000009770 ) ) ;
#9518 = DIRECTION ( 'NONE',  ( -0.000000000000000000, -0.000000000000000000, 1.000000000000000000 ) ) ;
#9519 = LINE ( 'NONE', #8029, #953 ) ;
#9520 = CARTESIAN_POINT ( 'NONE',  ( 4.000000000000000888, -7.851777359433979697, -3.255701506262516087 ) ) ;
#9521 = VERTEX_POINT ( 'NONE', #6191 ) ;
#9522 = DIRECTION ( 'NONE',  ( 1.000000000000000000, 0.000000000000000000, 0.000000000000000000 ) ) ;
#9523 = EDGE_CURVE ( 'NONE', #9197, #2891, #3020, .T. ) ;
#9524 = PLANE ( 'NONE',  #1706 ) ;
#9525 = CARTESIAN_POINT ( 'NONE',  ( -0.7401821875142701179, 4.673326407553649808, 10.77999999999999936 ) ) ;
#9526 = CARTESIAN_POINT ( 'NONE',  ( -1.500000000000000222, -13.00000000000000533, -1.750000000000000000 ) ) ;
#9527 = ORIENTED_EDGE ( 'NONE', *, *, #4025, .F. ) ;
#9528 = EDGE_CURVE ( 'NONE', #8329, #2528, #5801, .T. ) ;
#9529 = VERTEX_POINT ( 'NONE', #5554 ) ;
#9530 = CYLINDRICAL_SURFACE ( 'NONE', #1366, 1.500000000000000222 ) ;
#9531 = FILL_AREA_STYLE_COLOUR ( '', #8980 ) ;
#9532 = ORIENTED_EDGE ( 'NONE', *, *, #598, .T. ) ;
#9533 = CARTESIAN_POINT ( 'NONE',  ( 3.826313983664925811, 3.951860609387098044, 6.596051716722022285 ) ) ;
#9534 = LINE ( 'NONE', #8836, #6738 ) ;
#9535 = FACE_OUTER_BOUND ( 'NONE', #3696, .T. ) ;
#9536 = VERTEX_POINT ( 'NONE', #9550 ) ;
#9537 = DIRECTION ( 'NONE',  ( 0.000000000000000000, 0.000000000000000000, 1.000000000000000000 ) ) ;
#9538 = CARTESIAN_POINT ( 'NONE',  ( -2.542276634908081423, -5.195105386651227342, 13.45605171672202260 ) ) ;
#9539 = ORIENTED_EDGE ( 'NONE', *, *, #4965, .F. ) ;
#9540 = SURFACE_SIDE_STYLE ('',( #3851 ) ) ;
#9541 = DIRECTION ( 'NONE',  ( -0.9396926207859105373, 0.3420201433256627732, 0.000000000000000000 ) ) ;
#9542 = DIRECTION ( 'NONE',  ( 0.000000000000000000, 0.000000000000000000, 1.000000000000000000 ) ) ;
#9543 = VERTEX_POINT ( 'NONE', #8744 ) ;
#9544 = CARTESIAN_POINT ( 'NONE',  ( 3.889087296526005488, 3.889087296526018811, -3.866961113726609188E-17 ) ) ;
#9545 = CARTESIAN_POINT ( 'NONE',  ( 13.82973899676619745, -10.00000000000000000, -12.00000000000000000 ) ) ;
#9546 = CARTESIAN_POINT ( 'NONE',  ( 4.023224611898322145, -4.155232146225737111, 2.503948283277976472 ) ) ;
#9547 = ORIENTED_EDGE ( 'NONE', *, *, #2530, .F. ) ;
#9548 = CARTESIAN_POINT ( 'NONE',  ( -0.7500000000000007772, -14.29903810567666156, -1.729166668032260157 ) ) ;
#9549 = VECTOR ( 'NONE', #1725, 1000.000000000000000 ) ;
#9550 = CARTESIAN_POINT ( 'NONE',  ( 5.999999999999999112, -27.00000000000000711, -14.00000000000000178 ) ) ;
#9551 = EDGE_CURVE ( 'NONE', #2276, #10233, #3919, .T. ) ;
#9552 = EDGE_CURVE ( 'NONE', #3797, #7067, #4702, .T. ) ;
#9553 = EDGE_LOOP ( 'NONE', ( #9566, #9122, #7199 ) ) ;
#9554 = EDGE_CURVE ( 'NONE', #8006, #5123, #8691, .T. ) ;
#9555 = PRODUCT_DEFINITION_SHAPE ( 'NONE', 'NONE',  #10508 ) ;
#9556 = DIRECTION ( 'NONE',  ( 0.000000000000000000, 0.000000000000000000, -1.000000000000000000 ) ) ;
#9557 = CARTESIAN_POINT ( 'NONE',  ( 1.500000000000000222, -13.00000000000000533, -2.000000000000000000 ) ) ;
#9558 =( GEOMETRIC_REPRESENTATION_CONTEXT ( 3 ) GLOBAL_UNCERTAINTY_ASSIGNED_CONTEXT ( ( #465 ) ) GLOBAL_UNIT_ASSIGNED_CONTEXT ( ( #9812, #1596, #6560 ) ) REPRESENTATION_CONTEXT ( 'NONE', 'WORKASPACE' ) );
#9559 = CARTESIAN_POINT ( 'NONE',  ( 19.29399126966725575, 3.750000000000000000, -12.00000000000000000 ) ) ;
#9560 = DIRECTION ( 'NONE',  ( 0.000000000000000000, 0.000000000000000000, 1.000000000000000000 ) ) ;
#9561 = CARTESIAN_POINT ( 'NONE',  ( 2.042957248827968808, -4.009529358847652603, 6.439999999999999503 ) ) ;
#9562 = CARTESIAN_POINT ( 'NONE',  ( -0.6146835312499998594, -11.93533689329915326, -1.677083334016129967 ) ) ;
#9563 = CARTESIAN_POINT ( 'NONE',  ( 5.446173322633801384, 0.7727076532861675284, 10.48394828327797512 ) ) ;
#9564 = ADVANCED_FACE ( 'NONE', ( #10239 ), #1320, .F. ) ;
#9565 = CARTESIAN_POINT ( 'NONE',  ( -31.74999999999995737, 1.836970198721030181E-16, -1.500000000000000222 ) ) ;
#9566 = ORIENTED_EDGE ( 'NONE', *, *, #5334, .F. ) ;
#9567 = APPLICATION_PROTOCOL_DEFINITION ( 'draft international standard', 'automotive_design', 1998, #54 ) ;
#9568 = DIRECTION ( 'NONE',  ( 1.000000000000000000, -0.000000000000000000, -0.000000000000000000 ) ) ;
#9569 = PLANE ( 'NONE',  #4158 ) ;
#9570 = EDGE_LOOP ( 'NONE', ( #3067, #4847, #555, #2059 ) ) ;
#9571 = DIRECTION ( 'NONE',  ( -0.000000000000000000, -1.000000000000000000, -0.000000000000000000 ) ) ;
#9572 = CARTESIAN_POINT ( 'NONE',  ( 0.7499999999999991118, -14.29903810567666333, -1.583333333333333481 ) ) ;
#9573 = ORIENTED_EDGE ( 'NONE', *, *, #9829, .T. ) ;
#9574 = CARTESIAN_POINT ( 'NONE',  ( 9.000000000000000000, 19.99999999999999645, 15.00000000000000000 ) ) ;
#9575 = FILL_AREA_STYLE_COLOUR ( '', #1181 ) ;
#9576 = AXIS2_PLACEMENT_3D ( 'NONE', #10230, #2959, #9270 ) ;
#9577 = CARTESIAN_POINT ( 'NONE',  ( -2.042957248827969252, 4.009529358847651714, 7.839999999999999858 ) ) ;
#9578 = CARTESIAN_POINT ( 'NONE',  ( 1.060575238724907038E-16, -11.26794919243112680, -2.374999999999999556 ) ) ;
#9579 = PRODUCT_DEFINITION_FORMATION_WITH_SPECIFIED_SOURCE ( 'ANY', '', #7746, .NOT_KNOWN. ) ;
#9580 = ORIENTED_EDGE ( 'NONE', *, *, #7138, .T. ) ;
#9581 = ORIENTED_EDGE ( 'NONE', *, *, #1709, .T. ) ;
#9582 = DIRECTION ( 'NONE',  ( 0.000000000000000000, 3.819167204710539130E-14, -1.000000000000000000 ) ) ;
#9583 = VECTOR ( 'NONE', #623, 1000.000000000000000 ) ;
#9584 = LINE ( 'NONE', #8775, #354 ) ;
#9585 = VERTEX_POINT ( 'NONE', #6239 ) ;
#9586 = CARTESIAN_POINT ( 'NONE',  ( -0.6162731882459178134, -4.458484982038665834, 7.716051716722023279 ) ) ;
#9587 = DIRECTION ( 'NONE',  ( -1.000000000000000000, -0.000000000000000000, -0.000000000000000000 ) ) ;
#9588 = VERTEX_POINT ( 'NONE', #2173 ) ;
#9589 = LINE ( 'NONE', #7996, #8160 ) ;
#9590 = CARTESIAN_POINT ( 'NONE',  ( -0.6162731882459178134, -4.458484982038665834, 2.116051716722023190 ) ) ;
#9591 = AXIS2_PLACEMENT_3D ( 'NONE', #7645, #968, #7848 ) ;
#9592 = ORIENTED_EDGE ( 'NONE', *, *, #9551, .T. ) ;
#9593 = VECTOR ( 'NONE', #446, 1000.000000000000000 ) ;
#9594 = VERTEX_POINT ( 'NONE', #531 ) ;
#9595 = DIRECTION ( 'NONE',  ( -0.000000000000000000, -1.000000000000000000, -0.000000000000000000 ) ) ;
#9596 = DIRECTION ( 'NONE',  ( 0.000000000000000000, 0.000000000000000000, 1.000000000000000000 ) ) ;
#9597 = ORIENTED_EDGE ( 'NONE', *, *, #213, .F. ) ;
#9598 = CARTESIAN_POINT ( 'NONE',  ( -2.000000000000000000, -8.497168642645963388, -0.2193742428685764301 ) ) ;
#9599 = CARTESIAN_POINT ( 'NONE',  ( 4.432609873715410487, -11.61333805414684761, 0.000000000000000000 ) ) ;
#9600 = CARTESIAN_POINT ( 'NONE',  ( 5.697241258616385196, -0.9968613283357656840, 5.023948283277976046 ) ) ;
#9601 = ORIENTED_EDGE ( 'NONE', *, *, #7477, .F. ) ;
#9602 = CARTESIAN_POINT ( 'NONE',  ( 1.500000000000000222, -13.00000000000000533, -1.562500001365593416 ) ) ;
#9603 = ADVANCED_FACE ( 'NONE', ( #579 ), #4766, .F. ) ;
#9604 = CARTESIAN_POINT ( 'NONE',  ( -15.00000000000000000, 19.99999999999999645, -9.000000000000000000 ) ) ;
#9605 = CARTESIAN_POINT ( 'NONE',  ( -2.000000000000000000, 0.000000000000000000, 0.000000000000000000 ) ) ;
#9606 = ORIENTED_EDGE ( 'NONE', *, *, #5429, .T. ) ;
#9607 = FACE_OUTER_BOUND ( 'NONE', #5417, .T. ) ;
#9608 = FACE_OUTER_BOUND ( 'NONE', #10172, .T. ) ;
#9609 = CARTESIAN_POINT ( 'NONE',  ( -2.000000000000000000, 2.429606751577122026, -5.757344182232885466 ) ) ;
#9610 = DIRECTION ( 'NONE',  ( -1.000000000000000000, 0.000000000000000000, -0.000000000000000000 ) ) ;
#9611 =( REPRESENTATION_RELATIONSHIP ('NONE','NONE', #5100, #9732 ) REPRESENTATION_RELATIONSHIP_WITH_TRANSFORMATION ( #8181 )SHAPE_REPRESENTATION_RELATIONSHIP( ) );
#9612 = DIRECTION ( 'NONE',  ( 0.000000000000000000, 0.000000000000000000, -1.000000000000000000 ) ) ;
#9613 = CARTESIAN_POINT ( 'NONE',  ( -0.7401821875142701179, 4.673326407553649808, 10.77999999999999936 ) ) ;
#9614 = EDGE_CURVE ( 'NONE', #7286, #3593, #3074, .T. ) ;
#9615 = ADVANCED_FACE ( 'NONE', ( #1426 ), #7900, .T. ) ;
#9616 = CARTESIAN_POINT ( 'NONE',  ( 5.999999999999999112, 26.99999999999999289, 3.000000000000000000 ) ) ;
#9617 = VECTOR ( 'NONE', #9345, 1000.000000000000000 ) ;
#9618 = CARTESIAN_POINT ( 'NONE',  ( 3.889087296526005488, 3.889087296526018811, -3.866961113726609188E-17 ) ) ;
#9619 = LINE ( 'NONE', #10303, #3779 ) ;
#9620 = ORIENTED_EDGE ( 'NONE', *, *, #3734, .F. ) ;
#9621 = APPLICATION_PROTOCOL_DEFINITION ( 'draft international standard', 'automotive_design', 1998, #9064 ) ;
#9622 = PLANE ( 'NONE',  #6678 ) ;
#9623 = LINE ( 'NONE', #6416, #1963 ) ;
#9624 = ORIENTED_EDGE ( 'NONE', *, *, #2996, .T. ) ;
#9625 = DIRECTION ( 'NONE',  ( 1.000000000000000000, 1.156482317317871478E-16, -5.204170427930421283E-15 ) ) ;
#9626 = DIRECTION ( 'NONE',  ( -1.000000000000000000, 0.000000000000000000, -0.000000000000000000 ) ) ;
#9627 = FACE_OUTER_BOUND ( 'NONE', #9553, .T. ) ;
#9628 = EDGE_CURVE ( 'NONE', #1061, #1639, #1493, .T. ) ;
#9629 = FACE_OUTER_BOUND ( 'NONE', #9118, .T. ) ;
#9630 = DIRECTION ( 'NONE',  ( -0.000000000000000000, -0.000000000000000000, 1.000000000000000000 ) ) ;
#9631 = CARTESIAN_POINT ( 'NONE',  ( 4.458484982038663169, 0.6162731882459350219, -0.7160517167220232793 ) ) ;
#9632 = CARTESIAN_POINT ( 'NONE',  ( -1.500000000000000222, -13.00000000000000533, -2.250000000000000444 ) ) ;
#9633 = ADVANCED_FACE ( 'NONE', ( #5395, #4546 ), #4960, .F. ) ;
#9634 = ORIENTED_EDGE ( 'NONE', *, *, #8689, .T. ) ;
#9635 = VERTEX_POINT ( 'NONE', #143 ) ;
#9636 = LINE ( 'NONE', #10491, #10021 ) ;
#9637 = DIRECTION ( 'NONE',  ( 0.000000000000000000, 0.000000000000000000, -1.000000000000000000 ) ) ;
#9638 = EDGE_LOOP ( 'NONE', ( #5581, #821, #1000, #5071 ) ) ;
#9639 = FACE_OUTER_BOUND ( 'NONE', #7012, .T. ) ;
#9640 = CARTESIAN_POINT ( 'NONE',  ( 16.97133164676619899, 6.000000000000000888, -12.00000000000000000 ) ) ;
#9641 = ORIENTED_EDGE ( 'NONE', *, *, #7353, .T. ) ;
#9642 = LINE ( 'NONE', #10328, #5432 ) ;
#9643 = CARTESIAN_POINT ( 'NONE',  ( -3.119207202478379681, -3.244753828200550139, 2.396051716722022551 ) ) ;
#9644 = ORIENTED_EDGE ( 'NONE', *, *, #9331, .T. ) ;
#9645 = ORIENTED_EDGE ( 'NONE', *, *, #10327, .T. ) ;
#9646 = CARTESIAN_POINT ( 'NONE',  ( -5.999999999999999112, -27.00000000000000711, -4.000000000000000000 ) ) ;
#9647 = ADVANCED_FACE ( 'NONE', ( #2680 ), #6547, .T. ) ;
#9648 = VECTOR ( 'NONE', #7260, 1000.000000000000000 ) ;
#9649 = DIRECTION ( 'NONE',  ( 1.000000000000000000, 0.000000000000000000, 0.000000000000000000 ) ) ;
#9650 = VERTEX_POINT ( 'NONE', #9957 ) ;
#9651 = CARTESIAN_POINT ( 'NONE',  ( -5.711843387010018702, 0.9046671180729746187, 7.419999999999998153 ) ) ;
#9652 = CARTESIAN_POINT ( 'NONE',  ( -2.000000000000024425, 15.00000000000000355, -5.999999999999988454 ) ) ;
#9653 = CARTESIAN_POINT ( 'NONE',  ( 5.195105386651219348, 2.542276634908100075, 7.543948283277975619 ) ) ;
#9654 = VERTEX_POINT ( 'NONE', #8360 ) ;
#9655 = CARTESIAN_POINT ( 'NONE',  ( -3.181725716174720498E-16, -14.73205080756888385, -1.187500001365593638 ) ) ;
#9656 = EDGE_CURVE ( 'NONE', #9420, #6021, #3425, .T. ) ;
#9657 = CARTESIAN_POINT ( 'NONE',  ( 2.697157280332745266, 3.750000000000000000, 0.000000000000000000 ) ) ;
#9658 = VECTOR ( 'NONE', #7786, 1000.000000000000000 ) ;
#9659 = ORIENTED_EDGE ( 'NONE', *, *, #83, .T. ) ;
#9660 = DIRECTION ( 'NONE',  ( -0.5000000000000034417, 1.060575238724904696E-16, -0.8660254037844367092 ) ) ;
#9661 = EDGE_CURVE ( 'NONE', #3049, #5860, #9857, .T. ) ;
#9662 = DIRECTION ( 'NONE',  ( -0.000000000000000000, -0.000000000000000000, -1.000000000000000000 ) ) ;
#9663 = CARTESIAN_POINT ( 'NONE',  ( 0.000000000000000000, -13.00000000000000533, -3.000000000000000000 ) ) ;
#9664 = DIRECTION ( 'NONE',  ( -0.000000000000000000, 1.000000000000000000, -0.000000000000000000 ) ) ;
#9665 = AXIS2_PLACEMENT_3D ( 'NONE', #6767, #1856, #1003 ) ;
#9666 = CARTESIAN_POINT ( 'NONE',  ( 5.838749930332745919, 3.750000000000000000, 0.000000000000000000 ) ) ;
#9667 = CARTESIAN_POINT ( 'NONE',  ( -0.7401821875142701179, 4.673326407553649808, 7.979999999999999538 ) ) ;
#9668 = ORIENTED_EDGE ( 'NONE', *, *, #2748, .T. ) ;
#9669 = CARTESIAN_POINT ( 'NONE',  ( 0.6146835312499993043, -14.06466310670085562, -0.9270833340161300784 ) ) ;
#9670 = CARTESIAN_POINT ( 'NONE',  ( 5.195105386651219348, 2.542276634908100075, 7.543948283277975619 ) ) ;
#9671 = CARTESIAN_POINT ( 'NONE',  ( 13.83898384071655840, -10.02539999999999942, 0.000000000000000000 ) ) ;
#9672 = AXIS2_PLACEMENT_3D ( 'NONE', #3965, #7194, #4643 ) ;
#9673 = ORIENTED_EDGE ( 'NONE', *, *, #6523, .T. ) ;
#9674 = APPLICATION_PROTOCOL_DEFINITION ( 'draft international standard', 'automotive_design', 1998, #2357 ) ;
#9675 = AXIS2_PLACEMENT_3D ( 'NONE', #7001, #2933, #8657 ) ;
#9676 = CARTESIAN_POINT ( 'NONE',  ( 4.089228379062037178, -4.089228379062022967, 0.6999999999999997335 ) ) ;
#9677 = AXIS2_PLACEMENT_3D ( 'NONE', #9616, #3242, #5716 ) ;
#9678 = EDGE_CURVE ( 'NONE', #10224, #3169, #7455, .T. ) ;
#9679 = DIRECTION ( 'NONE',  ( 0.000000000000000000, 0.000000000000000000, -1.000000000000000000 ) ) ;
#9680 = VERTEX_POINT ( 'NONE', #5897 ) ;
#9681 = CARTESIAN_POINT ( 'NONE',  ( 0.1499999999999973577, 0.000000000000000000, 0.000000000000000000 ) ) ;
#9682 = CARTESIAN_POINT ( 'NONE',  ( 5.019816903233806471, 6.000000000000000000, 0.000000000000000000 ) ) ;
#9683 = CIRCLE ( 'NONE', #188, 6.248999999999999666 ) ;
#9684 = DIRECTION ( 'NONE',  ( -0.9396926207859105373, 0.3420201433256627732, 0.000000000000000000 ) ) ;
#9685 = VECTOR ( 'NONE', #6900, 1000.000000000000000 ) ;
#9686 = CARTESIAN_POINT ( 'NONE',  ( -5.999999999999999112, -27.00000000000000711, 3.000000000000000000 ) ) ;
#9687 = PLANE ( 'NONE',  #183 ) ;
#9688 = CARTESIAN_POINT ( 'NONE',  ( 4.444597532678119300, 0.7039550926810472786, 8.679999999999997939 ) ) ;
#9689 = CIRCLE ( 'NONE', #6446, 6.248999999999999666 ) ;
#9690 = CARTESIAN_POINT ( 'NONE',  ( -0.7500000000000007772, -14.29903810567666156, -1.166666666666666741 ) ) ;
#9691 = VERTEX_POINT ( 'NONE', #7558 ) ;
#9692 = AXIS2_PLACEMENT_3D ( 'NONE', #7759, #10208, #10103 ) ;
#9693 = EDGE_CURVE ( 'NONE', #9020, #10421, #6154, .T. ) ;
#9694 = EDGE_CURVE ( 'NONE', #6538, #3281, #2257, .T. ) ;
#9695 = ORIENTED_EDGE ( 'NONE', *, *, #8726, .F. ) ;
#9696 = CARTESIAN_POINT ( 'NONE',  ( 8.000000000000001776, 6.226349476952025341, -0.5315761383463619705 ) ) ;
#9697 = ORIENTED_EDGE ( 'NONE', *, *, #5738, .T. ) ;
#9698 = CARTESIAN_POINT ( 'NONE',  ( -0.7039550926810301812, -4.444597532678121965, 1.119999999999999885 ) ) ;
#9699 = LINE ( 'NONE', #8047, #1016 ) ;
#9700 = ORIENTED_EDGE ( 'NONE', *, *, #828, .F. ) ;
#9701 = CARTESIAN_POINT ( 'NONE',  ( 3.119207202478379681, 3.244753828200549695, 3.796051716722023350 ) ) ;
#9702 = VERTEX_POINT ( 'NONE', #1140 ) ;
#9703 = EDGE_CURVE ( 'NONE', #9040, #8624, #5746, .T. ) ;
#9704 =( NAMED_UNIT ( * ) PLANE_ANGLE_UNIT ( ) SI_UNIT ( $, .RADIAN. ) );
#9705 = CARTESIAN_POINT ( 'NONE',  ( -1.500000000000000222, -13.00000000000000533, -2.250000000000000444 ) ) ;
#9706 = PLANE ( 'NONE',  #2033 ) ;
#9707 = ORIENTED_EDGE ( 'NONE', *, *, #8514, .F. ) ;
#9708 = CARTESIAN_POINT ( 'NONE',  ( 5.711843387010018702, -0.9046671180729751738, 3.219999999999999751 ) ) ;
#9709 = DIRECTION ( 'NONE',  ( -1.000000000000000000, -0.000000000000000000, 0.000000000000000000 ) ) ;
#9710 = CARTESIAN_POINT ( 'NONE',  ( 5.446173322633801384, 0.7727076532861675284, 10.48394828327797512 ) ) ;
#9711 = ORIENTED_EDGE ( 'NONE', *, *, #2678, .F. ) ;
#9712 = CARTESIAN_POINT ( 'NONE',  ( -1.500000000000000000, -12.13397459621556607, -0.8541666680322602678 ) ) ;
#9713 = VERTEX_POINT ( 'NONE', #6747 ) ;
#9714 = PRODUCT ( 'cover', 'cover', '', ( #3246 ) ) ;
#9715 = CARTESIAN_POINT ( 'NONE',  ( 8.000000000000001776, 6.226349476952025341, 0.5315761383463611933 ) ) ;
#9716 = DIRECTION ( 'NONE',  ( 1.000000000000000000, 0.000000000000000000, 0.000000000000000000 ) ) ;
#9717 = DIRECTION ( 'NONE',  ( 1.000000000000000000, 0.000000000000000000, -0.000000000000000000 ) ) ;
#9718 = CARTESIAN_POINT ( 'NONE',  ( 10.00000000000000000, -5.979767908488852868, 1.814490771706165351 ) ) ;
#9719 = FACE_OUTER_BOUND ( 'NONE', #2360, .T. ) ;
#9720 = CARTESIAN_POINT ( 'NONE',  ( -3.244753828200538148, -3.119207202478392116, 3.203948283277977094 ) ) ;
#9721 = ORIENTED_EDGE ( 'NONE', *, *, #5870, .T. ) ;
#9722 = CARTESIAN_POINT ( 'NONE',  ( -0.6146835312500006365, -14.06466310670085562, -1.010416667349463227 ) ) ;
#9723 = CARTESIAN_POINT ( 'NONE',  ( -4.089228379062038066, 4.089228379062021190, 7.699999999999998401 ) ) ;
#9724 = CARTESIAN_POINT ( 'NONE',  ( 1.300000000000000044, 0.000000000000000000, 0.000000000000000000 ) ) ;
#9725 = AXIS2_PLACEMENT_3D ( 'NONE', #5048, #6731, #8928 ) ;
#9726 = PRODUCT_CONTEXT ( 'NONE', #6338, 'mechanical' ) ;
#9727 = CARTESIAN_POINT ( 'NONE',  ( 4.900535883036028828, -2.496947748567499126, 0.5599999999999999423 ) ) ;
#9728 = CARTESIAN_POINT ( 'NONE',  ( 1.229367062500000163, -13.00000000000000533, 0.1562499993172034307 ) ) ;
#9729 = CARTESIAN_POINT ( 'NONE',  ( 0.000000000000000000, -10.00000000000000000, -12.00000000000000000 ) ) ;
#9730 = CARTESIAN_POINT ( 'NONE',  ( 15.00000000000000000, 19.99999999999999645, -9.000000000000000000 ) ) ;
#9731 = DIRECTION ( 'NONE',  ( 1.000000000000000000, 0.000000000000000000, 0.000000000000000000 ) ) ;
#9732 = SHAPE_REPRESENTATION ( 'position sensor magnet', ( #2101 ), #581 ) ;
#9733 = CYLINDRICAL_SURFACE ( 'NONE', #9506, 2.500000000000000000 ) ;
#9734 = DIRECTION ( 'NONE',  ( 1.000000000000000000, -0.000000000000000000, -0.000000000000000000 ) ) ;
#9735 = CIRCLE ( 'NONE', #1085, 1.249999999999987121 ) ;
#9736 = EDGE_CURVE ( 'NONE', #8270, #4252, #3476, .T. ) ;
#9737 = CARTESIAN_POINT ( 'NONE',  ( 3.279728542977952799, -3.411736077305369541, 2.503948283277976472 ) ) ;
#9738 = CARTESIAN_POINT ( 'NONE',  ( 1.500000000000000222, -13.00000000000000533, -2.000000000000000000 ) ) ;
#9739 = ORIENTED_EDGE ( 'NONE', *, *, #4908, .F. ) ;
#9740 = PRESENTATION_LAYER_ASSIGNMENT (  '', '', ( #3974 ) ) ;
#9741 = EDGE_LOOP ( 'NONE', ( #1105, #6856, #8508, #3440 ) ) ;
#9742 = DIRECTION ( 'NONE',  ( 0.3420201433256627732, -0.9396926207859105373, 0.000000000000000000 ) ) ;
#9743 = DIRECTION ( 'NONE',  ( 0.000000000000000000, 0.000000000000000000, 1.000000000000000000 ) ) ;
#9744 = EDGE_LOOP ( 'NONE', ( #10496, #10131, #5167, #5950 ) ) ;
#9745 = VECTOR ( 'NONE', #3707, 1000.000000000000000 ) ;
#9746 = CARTESIAN_POINT ( 'NONE',  ( -3.181980515339458027, -3.181980515339470905, 4.200000000000000178 ) ) ;
#9747 = DIRECTION ( 'NONE',  ( -1.000000000000000000, -0.000000000000000000, 0.000000000000000000 ) ) ;
#9748 = VERTEX_POINT ( 'NONE', #5113 ) ;
#9749 = ADVANCED_FACE ( 'NONE', ( #2582 ), #2174, .T. ) ;
#9750 = EDGE_CURVE ( 'NONE', #3589, #8741, #7871, .T. ) ;
#9751 =( GEOMETRIC_REPRESENTATION_CONTEXT ( 3 ) GLOBAL_UNCERTAINTY_ASSIGNED_CONTEXT ( ( #6917 ) ) GLOBAL_UNIT_ASSIGNED_CONTEXT ( ( #251, #1091, #3628 ) ) REPRESENTATION_CONTEXT ( 'NONE', 'WORKASPACE' ) );
#9752 = CARTESIAN_POINT ( 'NONE',  ( -4.940838830814703542, 2.417848759854245078, 11.35605171672202296 ) ) ;
#9753 = ORIENTED_EDGE ( 'NONE', *, *, #8044, .T. ) ;
#9754 = CONICAL_SURFACE ( 'NONE', #7876, 1.219500000000000028, 0.7853981633974680410 ) ;
#9755 = PLANE ( 'NONE',  #3805 ) ;
#9756 = CARTESIAN_POINT ( 'NONE',  ( 0.000000000000000000, 6.000000000000000000, -12.00000000000000000 ) ) ;
#9757 = VERTEX_POINT ( 'NONE', #2721 ) ;
#9758 = CARTESIAN_POINT ( 'NONE',  ( -4.089228379062038066, 4.089228379062021190, 2.099999999999999201 ) ) ;
#9759 = CARTESIAN_POINT ( 'NONE',  ( 3.535533905932731980, 3.535533905932744414, 13.99999999999999822 ) ) ;
#9760 = CARTESIAN_POINT ( 'NONE',  ( 3.951860609387084722, 3.826313983664940022, 13.00394828327797470 ) ) ;
#9761 = VERTEX_POINT ( 'NONE', #6537 ) ;
#9762 = EDGE_CURVE ( 'NONE', #7181, #6915, #9787, .T. ) ;
#9763 = CARTESIAN_POINT ( 'NONE',  ( 1.500000000000000000, -13.86602540378444459, -0.1041666680322603095 ) ) ;
#9764 = CIRCLE ( 'NONE', #10100, 2.000000000000000000 ) ;
#9765 = ORIENTED_EDGE ( 'NONE', *, *, #1057, .T. ) ;
#9766 = LINE ( 'NONE', #7571, #1433 ) ;
#9767 = VECTOR ( 'NONE', #7273, 1000.000000000000000 ) ;
#9768 = CARTESIAN_POINT ( 'NONE',  ( 4.000000000000000000, -13.00000000000000533, 2.000000000000000000 ) ) ;
#9769 = DIRECTION ( 'NONE',  ( 1.000000000000000000, 0.000000000000000000, 0.000000000000000000 ) ) ;
#9770 = CARTESIAN_POINT ( 'NONE',  ( 20.72778015323380885, -10.00000000000000000, 0.000000000000000000 ) ) ;
#9771 = VECTOR ( 'NONE', #9610, 1000.000000000000000 ) ;
#9772 = LINE ( 'NONE', #4772, #9648 ) ;
#9773 = CARTESIAN_POINT ( 'NONE',  ( 4.444597532678119300, 0.7039550926810472786, 11.47999999999999865 ) ) ;
#9774 = EDGE_LOOP ( 'NONE', ( #9364, #10156, #7295, #9159 ) ) ;
#9775 = CARTESIAN_POINT ( 'NONE',  ( -1.229367062500000163, -12.29022459553277002, -0.6354166673494632267 ) ) ;
#9776 = CARTESIAN_POINT ( 'NONE',  ( 3.889087296526005488, 3.889087296526018811, 8.400000000000000355 ) ) ;
#9777 = DIRECTION ( 'NONE',  ( 0.000000000000000000, 0.000000000000000000, 1.000000000000000000 ) ) ;
#9778 = CARTESIAN_POINT ( 'NONE',  ( 0.000000000000000000, 6.000000000000000000, 0.000000000000000000 ) ) ;
#9779 = CARTESIAN_POINT ( 'NONE',  ( 0.000000000000000000, -4.000000000000000000, -12.00000000000000000 ) ) ;
#9780 = PLANE ( 'NONE',  #2978 ) ;
#9781 = FACE_OUTER_BOUND ( 'NONE', #1505, .T. ) ;
#9782 = CARTESIAN_POINT ( 'NONE',  ( 20.71853530928344611, -10.02539999999999942, -12.00000000000000000 ) ) ;
#9783 = CARTESIAN_POINT ( 'NONE',  ( -2.122056237541221968, 3.969226411068977889, 3.236051716722023297 ) ) ;
#9784 = CARTESIAN_POINT ( 'NONE',  ( 10.00000000000000000, 0.000000000000000000, 0.000000000000000000 ) ) ;
#9785 = CARTESIAN_POINT ( 'NONE',  ( 3.279728542977952799, -3.411736077305369541, 5.303948283277975406 ) ) ;
#9786 = EDGE_CURVE ( 'NONE', #3241, #247, #4201, .T. ) ;
#9787 = LINE ( 'NONE', #3357, #9549 ) ;
#9788 = ORIENTED_EDGE ( 'NONE', *, *, #10446, .F. ) ;
#9789 = ORIENTED_EDGE ( 'NONE', *, *, #6082, .T. ) ;
#9790 = LINE ( 'NONE', #5842, #2057 ) ;
#9791 = EDGE_CURVE ( 'NONE', #1449, #4422, #4615, .T. ) ;
#9792 = DIRECTION ( 'NONE',  ( 0.3420201433256627732, -0.9396926207859105373, 0.000000000000000000 ) ) ;
#9793 = ORIENTED_EDGE ( 'NONE', *, *, #9914, .F. ) ;
#9794 = CARTESIAN_POINT ( 'NONE',  ( 4.444597532678119300, 0.7039550926810472786, 3.079999999999999627 ) ) ;
#9795 = CARTESIAN_POINT ( 'NONE',  ( 19.29399126966725575, 3.750000000000000000, -12.00000000000000000 ) ) ;
#9796 = ORIENTED_EDGE ( 'NONE', *, *, #2279, .T. ) ;
#9797 = CARTESIAN_POINT ( 'NONE',  ( -0.6162731882459178134, -4.458484982038665834, 10.51605171672202133 ) ) ;
#9798 = PRODUCT_DEFINITION_SHAPE ( 'NONE', 'NONE',  #10505 ) ;
#9799 = CARTESIAN_POINT ( 'NONE',  ( 10.00000000000000000, 0.000000000000000000, 0.000000000000000000 ) ) ;
#9800 = ORIENTED_EDGE ( 'NONE', *, *, #4097, .T. ) ;
#9801 = ORIENTED_EDGE ( 'NONE', *, *, #7995, .T. ) ;
#9802 = EDGE_CURVE ( 'NONE', #1645, #2644, #5465, .T. ) ;
#9803 = CARTESIAN_POINT ( 'NONE',  ( -29.99999999999998934, -35.00000000000000000, 9.000000000000000000 ) ) ;
#9804 = EDGE_CURVE ( 'NONE', #3277, #9040, #2441, .T. ) ;
#9805 = LINE ( 'NONE', #5021, #10344 ) ;
#9806 = VERTEX_POINT ( 'NONE', #6638 ) ;
#9807 = CARTESIAN_POINT ( 'NONE',  ( -5.711843387010018702, 0.9046671180729746187, 4.620000000000000107 ) ) ;
#9808 = CARTESIAN_POINT ( 'NONE',  ( 4.089228379062037178, -4.089228379062022967, 6.299999999999999822 ) ) ;
#9809 = CARTESIAN_POINT ( 'NONE',  ( 2.496947748567516889, -4.900535883036019946, 3.639999999999999680 ) ) ;
#9810 = EDGE_LOOP ( 'NONE', ( #5684, #3955, #9788, #7349 ) ) ;
#9811 = CARTESIAN_POINT ( 'NONE',  ( -1.229367062500000163, -12.29022459553277002, -2.510416667349463449 ) ) ;
#9812 =( LENGTH_UNIT ( ) NAMED_UNIT ( * ) SI_UNIT ( .MILLI., .METRE. ) );
#9813 = ORIENTED_EDGE ( 'NONE', *, *, #2708, .T. ) ;
#9814 = EDGE_CURVE ( 'NONE', #4115, #7985, #6479, .T. ) ;
#9815 = CARTESIAN_POINT ( 'NONE',  ( 0.000000000000000000, -10.00000000000000000, 0.000000000000000000 ) ) ;
#9816 = CARTESIAN_POINT ( 'NONE',  ( 0.000000000000000000, 18.99999999999999289, 1.249999999999997558 ) ) ;
#9817 = DIRECTION ( 'NONE',  ( -0.000000000000000000, -0.000000000000000000, 1.000000000000000000 ) ) ;
#9818 = FACE_OUTER_BOUND ( 'NONE', #3075, .T. ) ;
#9819 = CARTESIAN_POINT ( 'NONE',  ( -0.6146835312499998594, -11.93533689329915326, -1.177083334016129967 ) ) ;
#9820 = CARTESIAN_POINT ( 'NONE',  ( 4.658724279160018966, -0.8323763977770426425, -0.5760517167220230439 ) ) ;
#9821 = VERTEX_POINT ( 'NONE', #8194 ) ;
#9822 = VECTOR ( 'NONE', #2629, 1000.000000000000000 ) ;
#9823 = CARTESIAN_POINT ( 'NONE',  ( -0.6146835312500006365, -14.06466310670085562, -0.5104166673494635598 ) ) ;
#9824 = VECTOR ( 'NONE', #7481, 1000.000000000000000 ) ;
#9825 = CARTESIAN_POINT ( 'NONE',  ( 3.889087296526005488, 3.889087296526018811, 5.599999999999998757 ) ) ;
#9826 = LINE ( 'NONE', #2558, #747 ) ;
#9827 = AXIS2_PLACEMENT_3D ( 'NONE', #9836, #1614, #5780 ) ;
#9828 = CONTEXT_DEPENDENT_SHAPE_REPRESENTATION ( #7428, #1663 ) ;
#9829 = EDGE_CURVE ( 'NONE', #2344, #7761, #61, .T. ) ;
#9830 = CARTESIAN_POINT ( 'NONE',  ( 5.711843387010019590, -0.9046671180729753958, 8.820000000000000284 ) ) ;
#9831 = VECTOR ( 'NONE', #2601, 1000.000000000000000 ) ;
#9832 = DIRECTION ( 'NONE',  ( 0.000000000000000000, 0.000000000000000000, -1.000000000000000000 ) ) ;
#9833 = PRESENTATION_LAYER_ASSIGNMENT (  '', '', ( #8470 ) ) ;
#9834 = CARTESIAN_POINT ( 'NONE',  ( 10.00000000000000000, 6.100541242131515496, 3.528937025535514138 ) ) ;
#9835 = CARTESIAN_POINT ( 'NONE',  ( 30.00000000000001066, 0.000000000000000000, 0.000000000000000000 ) ) ;
#9836 = CARTESIAN_POINT ( 'NONE',  ( 8.000000000000001776, -6.700937042937042065, -2.183447440113260196 ) ) ;
#9837 = CARTESIAN_POINT ( 'NONE',  ( 4.049832306626335310, -1.963858260114701215, 7.156051716722023670 ) ) ;
#9838 = CARTESIAN_POINT ( 'NONE',  ( -26.99999999999998934, -35.00000000000000000, 5.999999999999999112 ) ) ;
#9839 = AXIS2_PLACEMENT_3D ( 'NONE', #3430, #9910, #6705 ) ;
#9840 = CARTESIAN_POINT ( 'NONE',  ( 4.258245684917310037, 2.064922774268912686, 7.543948283277975619 ) ) ;
#9841 = AXIS2_PLACEMENT_3D ( 'NONE', #4891, #6424, #10484 ) ;
#9842 = DIRECTION ( 'NONE',  ( 0.000000000000000000, 0.000000000000000000, 1.000000000000000000 ) ) ;
#9843 = EDGE_LOOP ( 'NONE', ( #7299, #1090, #3795, #5966 ) ) ;
#9844 = CARTESIAN_POINT ( 'NONE',  ( 2.576046737280769605, -4.860232935257343456, 4.636051716722022320 ) ) ;
#9845 = ORIENTED_EDGE ( 'NONE', *, *, #4946, .F. ) ;
#9846 = ADVANCED_FACE ( 'NONE', ( #1877, #3415, #8984 ), #82, .F. ) ;
#9847 = PLANE ( 'NONE',  #532 ) ;
#9848 = DIRECTION ( 'NONE',  ( 0.000000000000000000, 0.000000000000000000, 1.000000000000000000 ) ) ;
#9849 = EDGE_CURVE ( 'NONE', #3187, #5332, #2516, .T. ) ;
#9850 = VERTEX_POINT ( 'NONE', #7496 ) ;
#9851 = CARTESIAN_POINT ( 'NONE',  ( -4.215868657802586128, -2.148092372876348133, 1.540000000000000036 ) ) ;
#9852 = VECTOR ( 'NONE', #526, 1000.000000000000000 ) ;
#9853 = CARTESIAN_POINT ( 'NONE',  ( -2.000000000000000000, 0.000000000000000000, 0.000000000000000000 ) ) ;
#9854 = ORIENTED_EDGE ( 'NONE', *, *, #6108, .F. ) ;
#9855 = CARTESIAN_POINT ( 'NONE',  ( 2.122056237541221524, -3.969226411068978777, 10.23605171672202374 ) ) ;
#9856 = AXIS2_PLACEMENT_3D ( 'NONE', #8517, #1251, #6965 ) ;
#9857 = LINE ( 'NONE', #5850, #6817 ) ;
#9858 = EDGE_CURVE ( 'NONE', #4568, #7564, #132, .T. ) ;
#9859 = ORIENTED_EDGE ( 'NONE', *, *, #8455, .T. ) ;
#9860 = EDGE_LOOP ( 'NONE', ( #5611, #9311, #4430, #7789 ) ) ;
#9861 = CARTESIAN_POINT ( 'NONE',  ( 15.00000000000000000, 19.99999999999999645, 9.000000000000000000 ) ) ;
#9862 = CARTESIAN_POINT ( 'NONE',  ( -1.387778780781445991E-14, 15.00000000000000355, 0.000000000000000000 ) ) ;
#9863 = ORIENTED_EDGE ( 'NONE', *, *, #2948, .T. ) ;
#9864 = CARTESIAN_POINT ( 'NONE',  ( -0.9046671180729963790, 5.711843387010016926, 2.379999999999999893 ) ) ;
#9865 = CARTESIAN_POINT ( 'NONE',  ( -0.9480714621563718358, -5.418398423912716311, 11.32394828327797676 ) ) ;
#9866 = ORIENTED_EDGE ( 'NONE', *, *, #6801, .F. ) ;
#9867 = CARTESIAN_POINT ( 'NONE',  ( 0.6146835312499993043, -14.06466310670085562, -1.802083334016129745 ) ) ;
#9868 = EDGE_CURVE ( 'NONE', #3947, #317, #4153, .T. ) ;
#9869 = ORIENTED_EDGE ( 'NONE', *, *, #7115, .T. ) ;
#9870 = CARTESIAN_POINT ( 'NONE',  ( 0.000000000000000000, 6.000000000000000000, -12.00000000000000000 ) ) ;
#9871 = DIRECTION ( 'NONE',  ( 0.3420201433256627732, -0.9396926207859105373, 0.000000000000000000 ) ) ;
#9872 = CARTESIAN_POINT ( 'NONE',  ( 7.555798540716556211, -10.02539999999999942, -12.00000000000000000 ) ) ;
#9873 = EDGE_LOOP ( 'NONE', ( #1561, #98, #8962 ) ) ;
#9874 = DIRECTION ( 'NONE',  ( 0.000000000000000000, 0.000000000000000000, -1.000000000000000000 ) ) ;
#9875 = CARTESIAN_POINT ( 'NONE',  ( -2.607672531582950546E-16, -14.41955080893447416, -2.468750000682796930 ) ) ;
#9876 = CARTESIAN_POINT ( 'NONE',  ( 4.458484982038663169, 0.6162731882459350219, -0.7160517167220232793 ) ) ;
#9877 = ORIENTED_EDGE ( 'NONE', *, *, #8700, .F. ) ;
#9878 = CARTESIAN_POINT ( 'NONE',  ( 17.00000000000000000, 19.99999999999999645, 9.000000000000000000 ) ) ;
#9879 = EDGE_CURVE ( 'NONE', #252, #9588, #741, .T. ) ;
#9880 = EDGE_CURVE ( 'NONE', #9594, #5863, #4738, .T. ) ;
#9881 = CARTESIAN_POINT ( 'NONE',  ( 5.432285873273257515, 0.8603895577212793411, 3.079999999999999627 ) ) ;
#9882 = DIRECTION ( 'NONE',  ( 0.000000000000000000, 0.000000000000000000, 1.000000000000000000 ) ) ;
#9883 = CARTESIAN_POINT ( 'NONE',  ( 5.711843387010019590, -0.9046671180729753958, 6.019999999999999574 ) ) ;
#9884 = AXIS2_PLACEMENT_3D ( 'NONE', #8685, #8484, #1370 ) ;
#9885 = CARTESIAN_POINT ( 'NONE',  ( 0.000000000000000000, 0.000000000000000000, -10.00000000000000000 ) ) ;
#9886 = DIRECTION ( 'NONE',  ( 1.000000000000000000, 0.000000000000000000, 0.000000000000000000 ) ) ;
#9887 = PLANE ( 'NONE',  #9399 ) ;
#9888 = CARTESIAN_POINT ( 'NONE',  ( -4.155232146225753098, 4.023224611898306158, 14.29605171672202424 ) ) ;
#9889 = CARTESIAN_POINT ( 'NONE',  ( -1.229367062500000385, -13.70977540446723886, -0.9270833340161298564 ) ) ;
#9890 = ADVANCED_FACE ( 'NONE', ( #7704 ), #441, .F. ) ;
#9891 = CARTESIAN_POINT ( 'NONE',  ( -1.963858260114716980, 4.049832306626327316, 9.643948283277975264 ) ) ;
#9892 = AXIS2_PLACEMENT_3D ( 'NONE', #1772, #4949, #5729 ) ;
#9893 = DIRECTION ( 'NONE',  ( 0.3420201433256627732, -0.9396926207859105373, 0.000000000000000000 ) ) ;
#9894 = ORIENTED_EDGE ( 'NONE', *, *, #3079, .T. ) ;
#9895 = CARTESIAN_POINT ( 'NONE',  ( 5.418398423912711870, 0.9480714621563913758, 1.276051716722023333 ) ) ;
#9896 = CARTESIAN_POINT ( 'NONE',  ( 30.00000000000001066, 35.00000000000001421, 9.000000000000000000 ) ) ;
#9897 = CARTESIAN_POINT ( 'NONE',  ( -1.500000000000000222, -13.00000000000000533, -2.750000000000000000 ) ) ;
#9898 = ORIENTED_EDGE ( 'NONE', *, *, #8502, .T. ) ;
#9899 = AXIS2_PLACEMENT_3D ( 'NONE', #1012, #4882, #862 ) ;
#9900 = LINE ( 'NONE', #4208, #9822 ) ;
#9901 = DIRECTION ( 'NONE',  ( 1.000000000000000000, 0.000000000000000000, 0.000000000000000000 ) ) ;
#9902 = VERTEX_POINT ( 'NONE', #6895 ) ;
#9903 = CARTESIAN_POINT ( 'NONE',  ( -3.119207202478379681, -3.244753828200550139, 7.996051716722022640 ) ) ;
#9904 = DIRECTION ( 'NONE',  ( -0.000000000000000000, -0.000000000000000000, 1.000000000000000000 ) ) ;
#9905 = EDGE_LOOP ( 'NONE', ( #147, #3882, #463, #549, #4681, #857, #6121, #5685, #1406, #6539, #589, #6706, #6591, #600, #8481, #6859, #10469, #4578, #490, #10493, #6483, #7625, #443, #3975, #2485, #8217, #7358, #3360, #9753, #10261, #3596, #10304, #8532, #9800, #10309, #6150 ) ) ;
#9906 = PRODUCT_DEFINITION ( 'UNKNOWN', '', #7872, #3152 ) ;
#9907 = VECTOR ( 'NONE', #6982, 1000.000000000000000 ) ;
#9908 = ORIENTED_EDGE ( 'NONE', *, *, #4152, .T. ) ;
#9909 = DIRECTION ( 'NONE',  ( 0.000000000000000000, 0.000000000000000000, 1.000000000000000000 ) ) ;
#9910 = DIRECTION ( 'NONE',  ( 0.000000000000000000, 0.000000000000000000, 1.000000000000000000 ) ) ;
#9911 = ORIENTED_EDGE ( 'NONE', *, *, #4178, .T. ) ;
#9912 = CARTESIAN_POINT ( 'NONE',  ( -2.576046737280769605, 4.860232935257343456, 3.236051716722023297 ) ) ;
#9913 = CARTESIAN_POINT ( 'NONE',  ( -2.625446233515515981, -5.152728359536500768, 6.859999999999999432 ) ) ;
#9914 = EDGE_CURVE ( 'NONE', #5526, #928, #10149, .T. ) ;
#9915 = CARTESIAN_POINT ( 'NONE',  ( 5.152728359536493663, 2.625446233515533745, 8.539999999999999147 ) ) ;
#9916 = ORIENTED_EDGE ( 'NONE', *, *, #4908, .T. ) ;
#9917 = CARTESIAN_POINT ( 'NONE',  ( -0.6146835312499998594, -11.93533689329915326, -1.052083334016129967 ) ) ;
#9918 = CONICAL_SURFACE ( 'NONE', #7365, 1.280000000000000027, 1.047197551196593857 ) ;
#9919 = AXIS2_PLACEMENT_3D ( 'NONE', #4616, #303, #2739 ) ;
#9920 = ORIENTED_EDGE ( 'NONE', *, *, #8493, .T. ) ;
#9921 = DIRECTION ( 'NONE',  ( 1.000000000000000000, 0.000000000000000000, 0.000000000000000000 ) ) ;
#9922 = PLANE ( 'NONE',  #1205 ) ;
#9923 = LINE ( 'NONE', #2752, #4902 ) ;
#9924 = ORIENTED_EDGE ( 'NONE', *, *, #7662, .F. ) ;
#9925 = CARTESIAN_POINT ( 'NONE',  ( 1.300000000000000044, -1.314525273895014473E-15, -1.280000000000000027 ) ) ;
#9926 = VECTOR ( 'NONE', #99, 1000.000000000000000 ) ;
#9927 = ADVANCED_FACE ( 'NONE', ( #4613 ), #4779, .T. ) ;
#9928 = CARTESIAN_POINT ( 'NONE',  ( 8.692241771943170539E-17, -11.58044919106553650, -1.718750000682796708 ) ) ;
#9929 = CARTESIAN_POINT ( 'NONE',  ( -0.7916369971161423269, -4.430710083317576320, 0.1239482832779766203 ) ) ;
#9930 = VERTEX_POINT ( 'NONE', #3085 ) ;
#9931 = CYLINDRICAL_SURFACE ( 'NONE', #4924, 2.399999999999999911 ) ;
#9932 = CARTESIAN_POINT ( 'NONE',  ( -5.152728359536494551, -2.625446233515535077, 1.540000000000000036 ) ) ;
#9933 = CARTESIAN_POINT ( 'NONE',  ( 12.99999999999999645, 19.99999999999999645, -9.000000000000000000 ) ) ;
#9934 = VECTOR ( 'NONE', #868, 1000.000000000000114 ) ;
#9935 = CARTESIAN_POINT ( 'NONE',  ( 5.432285873273257515, 0.8603895577212793411, 11.47999999999999865 ) ) ;
#9936 = AXIS2_PLACEMENT_3D ( 'NONE', #6739, #2776, #5991 ) ;
#9937 = CARTESIAN_POINT ( 'NONE',  ( 16.98057649071655817, -10.02539999999999942, 0.000000000000000000 ) ) ;
#9938 = EDGE_CURVE ( 'NONE', #2255, #2670, #9619, .T. ) ;
#9939 = PLANE ( 'NONE',  #8402 ) ;
#9940 = EDGE_CURVE ( 'NONE', #9979, #317, #3031, .T. ) ;
#9941 = DIRECTION ( 'NONE',  ( -1.000000000000000000, -0.000000000000000000, -0.000000000000000000 ) ) ;
#9942 = CARTESIAN_POINT ( 'NONE',  ( -2.576046737280769605, 4.860232935257343456, 14.43605171672202125 ) ) ;
#9943 = CYLINDRICAL_SURFACE ( 'NONE', #2722, 2.000000000000000000 ) ;
#9944 = CARTESIAN_POINT ( 'NONE',  ( 3.244753828200538148, 3.119207202478391672, 1.803948283277976516 ) ) ;
#9945 = CARTESIAN_POINT ( 'NONE',  ( 1.229367062500000163, -13.70977540446723886, -2.260416667349463449 ) ) ;
#9946 = ORIENTED_EDGE ( 'NONE', *, *, #4254, .T. ) ;
#9947 = CARTESIAN_POINT ( 'NONE',  ( -0.7727076532861475444, -5.446173322633804048, 4.916051716722023457 ) ) ;
#9948 = ADVANCED_FACE ( 'NONE', ( #5409 ), #2343, .T. ) ;
#9949 = CARTESIAN_POINT ( 'NONE',  ( 7.555798540716556211, -10.02539999999999942, -12.00000000000000000 ) ) ;
#9950 = CARTESIAN_POINT ( 'NONE',  ( 5.999999999999999112, 26.99999999999999289, 3.000000000000000000 ) ) ;
#9951 = VERTEX_POINT ( 'NONE', #2984 ) ;
#9952 = CARTESIAN_POINT ( 'NONE',  ( 2.148092372876330369, 4.215868657802594122, 8.259999999999999787 ) ) ;
#9953 = APPLICATION_CONTEXT ( 'automotive_design' ) ;
#9954 =( NAMED_UNIT ( * ) PLANE_ANGLE_UNIT ( ) SI_UNIT ( $, .RADIAN. ) );
#9955 = EDGE_CURVE ( 'NONE', #10377, #4895, #7104, .T. ) ;
#9956 = CARTESIAN_POINT ( 'NONE',  ( 0.6162731882459174804, 4.458484982038668498, 11.91605171672202346 ) ) ;
#9957 = CARTESIAN_POINT ( 'NONE',  ( 15.26352788033274699, -7.750000000000000000, 0.000000000000000000 ) ) ;
#9958 = EDGE_LOOP ( 'NONE', ( #5077, #3416, #7600, #1558 ) ) ;
#9959 = DIRECTION ( 'NONE',  ( 0.000000000000000000, 0.000000000000000000, 1.000000000000000000 ) ) ;
#9960 = ORIENTED_EDGE ( 'NONE', *, *, #8079, .T. ) ;
#9961 = ADVANCED_FACE ( 'NONE', ( #6305 ), #3191, .T. ) ;
#9962 = CARTESIAN_POINT ( 'NONE',  ( -17.00000000000000000, 19.99999999999999645, -5.999999999999999112 ) ) ;
#9963 = CARTESIAN_POINT ( 'NONE',  ( 5.999999999999999112, 26.99999999999999289, 3.000000000000000000 ) ) ;
#9964 = ORIENTED_EDGE ( 'NONE', *, *, #8112, .T. ) ;
#9965 = CARTESIAN_POINT ( 'NONE',  ( 3.826313983664925811, 3.951860609387098044, 3.796051716722023350 ) ) ;
#9966 = CARTESIAN_POINT ( 'NONE',  ( 2.625446233515515537, 5.152728359536502545, 2.659999999999998366 ) ) ;
#9967 = CARTESIAN_POINT ( 'NONE',  ( -2.625446233515515981, -5.152728359536500768, 12.45999999999999552 ) ) ;
#9968 = ORIENTED_EDGE ( 'NONE', *, *, #10126, .F. ) ;
#9969 = CARTESIAN_POINT ( 'NONE',  ( -1.229367062500000163, -13.00000000000000533, -0.4687500006827967081 ) ) ;
#9970 = EDGE_CURVE ( 'NONE', #1402, #946, #6413, .T. ) ;
#9971 = ORIENTED_EDGE ( 'NONE', *, *, #7678, .F. ) ;
#9972 = DIRECTION ( 'NONE',  ( 0.3420201433256627732, 0.9396926207859105373, -0.000000000000000000 ) ) ;
#9973 = DIRECTION ( 'NONE',  ( 0.000000000000000000, 0.000000000000000000, 1.000000000000000000 ) ) ;
#9974 = VERTEX_POINT ( 'NONE', #2402 ) ;
#9975 = DIRECTION ( 'NONE',  ( 0.000000000000000000, 0.000000000000000000, -1.000000000000000000 ) ) ;
#9976 = CARTESIAN_POINT ( 'NONE',  ( -0.6146835312500006365, -14.06466310670085562, -0.5104166673494635598 ) ) ;
#9977 = ADVANCED_FACE ( 'NONE', ( #7268 ), #5566, .F. ) ;
#9978 = CARTESIAN_POINT ( 'NONE',  ( -3.969226411068985882, 2.122056237541205537, 12.16394828327797661 ) ) ;
#9979 = VERTEX_POINT ( 'NONE', #3822 ) ;
#9980 = EDGE_CURVE ( 'NONE', #8371, #3693, #7966, .T. ) ;
#9981 = DIRECTION ( 'NONE',  ( -0.000000000000000000, -0.000000000000000000, 1.000000000000000000 ) ) ;
#9982 = CARTESIAN_POINT ( 'NONE',  ( 0.9046671180729951578, -5.711843387010016926, 12.17999999999999439 ) ) ;
#9983 = FACE_OUTER_BOUND ( 'NONE', #4878, .T. ) ;
#9984 = EDGE_CURVE ( 'NONE', #3139, #6004, #3873, .T. ) ;
#9985 = CARTESIAN_POINT ( 'NONE',  ( 4.900535883036028828, -2.496947748567499126, 11.75999999999999979 ) ) ;
#9986 = PLANE ( 'NONE',  #6185 ) ;
#9987 = CARTESIAN_POINT ( 'NONE',  ( -0.7499999999999997780, -11.70096189432334555, -1.895833334698926897 ) ) ;
#9988 = VECTOR ( 'NONE', #722, 1000.000000000000000 ) ;
#9989 = CARTESIAN_POINT ( 'NONE',  ( 0.000000000000000000, 26.99999999999999289, 0.000000000000000000 ) ) ;
#9990 = CARTESIAN_POINT ( 'NONE',  ( -4.049832306626335310, 1.963858260114700327, 11.35605171672202296 ) ) ;
#9991 = VECTOR ( 'NONE', #10339, 1000.000000000000000 ) ;
#9992 = CARTESIAN_POINT ( 'NONE',  ( -2.607672531582950546E-16, -14.41955080893447416, -1.343750000682796708 ) ) ;
#9993 = CARTESIAN_POINT ( 'NONE',  ( -4.458484982038663169, -0.6162731882459353550, 11.88394828327797548 ) ) ;
#9994 = DIRECTION ( 'NONE',  ( -1.000000000000000000, 0.000000000000000000, 0.000000000000000000 ) ) ;
#9995 = AXIS2_PLACEMENT_3D ( 'NONE', #957, #9014, #5031 ) ;
#9996 = VERTEX_POINT ( 'NONE', #591 ) ;
#9997 = ADVANCED_FACE ( 'NONE', ( #7910 ), #8702, .T. ) ;
#9998 = PRESENTATION_LAYER_ASSIGNMENT (  '', '', ( #6249 ) ) ;
#9999 = CARTESIAN_POINT ( 'NONE',  ( 4.155232146225751322, -4.023224611898307934, 4.496051716722022640 ) ) ;
#10000 = CARTESIAN_POINT ( 'NONE',  ( 0.000000000000000000, 0.000000000000000000, -2.000000000000000000 ) ) ;
#10001 = CARTESIAN_POINT ( 'NONE',  ( 0.000000000000000000, -7.063614741696270016, 2.343061888689530026 ) ) ;
#10002 = ORIENTED_EDGE ( 'NONE', *, *, #2326, .T. ) ;
#10003 = VECTOR ( 'NONE', #4368, 1000.000000000000000 ) ;
#10004 = CARTESIAN_POINT ( 'NONE',  ( -0.7039550926810301812, -4.444597532678121965, 9.519999999999999574 ) ) ;
#10005 = CARTESIAN_POINT ( 'NONE',  ( -4.444597532678119300, -0.7039550926810477227, 1.679999999999999938 ) ) ;
#10006 = ADVANCED_FACE ( 'NONE', ( #2293 ), #5517, .T. ) ;
#10007 = CARTESIAN_POINT ( 'NONE',  ( -0.6146835312499998594, -11.93533689329915326, -2.177083334016129967 ) ) ;
#10008 = EDGE_CURVE ( 'NONE', #5295, #2931, #703, .T. ) ;
#10009 = ORIENTED_EDGE ( 'NONE', *, *, #654, .F. ) ;
#10010 = DIRECTION ( 'NONE',  ( 1.000000000000000000, 0.000000000000000000, 0.000000000000000000 ) ) ;
#10011 = CIRCLE ( 'NONE', #5091, 2.500000000000000000 ) ;
#10012 = ORIENTED_EDGE ( 'NONE', *, *, #7664, .F. ) ;
#10013 = LINE ( 'NONE', #6909, #3313 ) ;
#10014 = VECTOR ( 'NONE', #8503, 1000.000000000000000 ) ;
#10015 = APPLICATION_CONTEXT ( 'automotive_design' ) ;
#10016 = CIRCLE ( 'NONE', #5424, 8.500000000000000000 ) ;
#10017 = CARTESIAN_POINT ( 'NONE',  ( 0.000000000000000000, 0.000000000000000000, 0.000000000000000000 ) ) ;
#10018 = ORIENTED_EDGE ( 'NONE', *, *, #654, .T. ) ;
#10019 = CARTESIAN_POINT ( 'NONE',  ( 2.496947748567516889, -4.900535883036019946, 9.240000000000000213 ) ) ;
#10020 = CARTESIAN_POINT ( 'NONE',  ( 4.089228379062037178, -4.089228379062022967, 0.6999999999999997335 ) ) ;
#10021 = VECTOR ( 'NONE', #2256, 1000.000000000000000 ) ;
#10022 = CARTESIAN_POINT ( 'NONE',  ( 0.9046671180729951578, -5.711843387010016926, 6.579999999999999183 ) ) ;
#10023 = ORIENTED_EDGE ( 'NONE', *, *, #8293, .T. ) ;
#10024 = CARTESIAN_POINT ( 'NONE',  ( 1.229367062499999719, -13.70977540446724063, -0.2604166673494632822 ) ) ;
#10025 = ADVANCED_FACE ( 'NONE', ( #7158, #9512, #10416 ), #1389, .F. ) ;
#10026 = VECTOR ( 'NONE', #7075, 1000.000000000000000 ) ;
#10027 = CARTESIAN_POINT ( 'NONE',  ( 0.000000000000000000, 0.000000000000000000, 0.000000000000000000 ) ) ;
#10028 = VERTEX_POINT ( 'NONE', #170 ) ;
#10029 = VECTOR ( 'NONE', #6485, 1000.000000000000000 ) ;
#10030 = CARTESIAN_POINT ( 'NONE',  ( 4.000000000000000888, 8.265874651078018331, 1.981241088980807419 ) ) ;
#10031 = DIRECTION ( 'NONE',  ( 0.000000000000000000, 0.000000000000000000, 1.000000000000000000 ) ) ;
#10032 = ORIENTED_EDGE ( 'NONE', *, *, #9230, .T. ) ;
#10033 = DIRECTION ( 'NONE',  ( -0.7071067811865465735, -0.7071067811865483499, 0.000000000000000000 ) ) ;
#10034 = DIRECTION ( 'NONE',  ( 0.9396926207859105373, -0.3420201433256627732, 0.000000000000000000 ) ) ;
#10035 = CARTESIAN_POINT ( 'NONE',  ( 8.692241771943170539E-17, -11.58044919106553650, -2.218750000682796486 ) ) ;
#10036 = CARTESIAN_POINT ( 'NONE',  ( 3.244753828200538148, 3.119207202478391672, 10.20394828327797399 ) ) ;
#10037 = ORIENTED_EDGE ( 'NONE', *, *, #6848, .F. ) ;
#10038 = CARTESIAN_POINT ( 'NONE',  ( 11.29375735928344504, -10.02539999999999942, -12.00000000000000000 ) ) ;
#10039 = ADVANCED_FACE ( 'NONE', ( #3403, #8968 ), #8180, .F. ) ;
#10040 = DIRECTION ( 'NONE',  ( -2.312964634635742957E-16, 1.000000000000000000, 0.000000000000000000 ) ) ;
#10041 = DIRECTION ( 'NONE',  ( 1.000000000000000000, 0.000000000000000000, -0.000000000000000000 ) ) ;
#10042 = CARTESIAN_POINT ( 'NONE',  ( 5.711843387010019590, -0.9046671180729753958, 3.219999999999999751 ) ) ;
#10043 = CARTESIAN_POINT ( 'NONE',  ( 8.000000000000001776, 2.429606751577122026, -5.757344182232885466 ) ) ;
#10044 = CARTESIAN_POINT ( 'NONE',  ( 5.838749930332745919, -7.750000000000000000, -12.00000000000000000 ) ) ;
#10045 = FACE_OUTER_BOUND ( 'NONE', #7549, .T. ) ;
#10046 = CARTESIAN_POINT ( 'NONE',  ( -0.7401821875142701179, 4.673326407553649808, 2.379999999999999893 ) ) ;
#10047 = CARTESIAN_POINT ( 'NONE',  ( -1.229367062500000385, -13.70977540446723886, -2.427083334016129967 ) ) ;
#10048 = CARTESIAN_POINT ( 'NONE',  ( 3.279728542977952799, -3.411736077305369541, 10.90394828327797327 ) ) ;
#10049 = CARTESIAN_POINT ( 'NONE',  ( 8.692241771943170539E-17, -11.58044919106553650, -0.09375000068279679133 ) ) ;
#10050 = ORIENTED_EDGE ( 'NONE', *, *, #3777, .F. ) ;
#10051 = CARTESIAN_POINT ( 'NONE',  ( 3.826313983664925811, 3.951860609387098044, 3.796051716722023350 ) ) ;
#10052 = DIRECTION ( 'NONE',  ( 1.000000000000000000, 0.000000000000000000, 0.000000000000000000 ) ) ;
#10053 = FACE_OUTER_BOUND ( 'NONE', #6018, .T. ) ;
#10054 = ORIENTED_EDGE ( 'NONE', *, *, #2913, .T. ) ;
#10055 = EDGE_CURVE ( 'NONE', #10476, #3049, #1814, .T. ) ;
#10056 = CARTESIAN_POINT ( 'NONE',  ( 4.673326407553653361, -0.7401821875142525764, 8.820000000000000284 ) ) ;
#10057 = AXIS2_PLACEMENT_3D ( 'NONE', #2241, #10363, #3988 ) ;
#10058 =( NAMED_UNIT ( * ) SI_UNIT ( $, .STERADIAN. ) SOLID_ANGLE_UNIT ( ) );
#10059 = CARTESIAN_POINT ( 'NONE',  ( 0.7039550926810297371, 4.444597532678122853, 5.319999999999999396 ) ) ;
#10060 = CARTESIAN_POINT ( 'NONE',  ( -0.6146835312499998594, -11.93533689329915326, -1.677083334016129967 ) ) ;
#10061 = EDGE_LOOP ( 'NONE', ( #10123, #8885, #7998, #4850 ) ) ;
#10062 = EDGE_LOOP ( 'NONE', ( #6545, #4257, #5165, #2434 ) ) ;
#10063 = CARTESIAN_POINT ( 'NONE',  ( 0.000000000000000000, 6.000000000000000000, -12.00000000000000000 ) ) ;
#10064 = DIRECTION ( 'NONE',  ( -1.000000000000000000, 0.000000000000000000, 0.000000000000000000 ) ) ;
#10065 = EDGE_LOOP ( 'NONE', ( #4114, #1419, #8019, #9673 ) ) ;
#10066 = EDGE_CURVE ( 'NONE', #8624, #4919, #1242, .T. ) ;
#10067 = CARTESIAN_POINT ( 'NONE',  ( -4.940838830814703542, 2.417848759854245078, 2.956051716722023492 ) ) ;
#10068 = EDGE_CURVE ( 'NONE', #9442, #9691, #7160, .T. ) ;
#10069 = CARTESIAN_POINT ( 'NONE',  ( 4.089228379062037178, -4.089228379062022967, 9.099999999999999645 ) ) ;
#10070 = CARTESIAN_POINT ( 'NONE',  ( 5.711843387010018702, -0.9046671180729751738, 11.61999999999999922 ) ) ;
#10071 = ORIENTED_EDGE ( 'NONE', *, *, #9879, .F. ) ;
#10072 = CARTESIAN_POINT ( 'NONE',  ( 17.57694265928344635, 6.025400000000000311, -12.00000000000000000 ) ) ;
#10073 = AXIS2_PLACEMENT_3D ( 'NONE', #1482, #4654, #6988 ) ;
#10074 = ORIENTED_EDGE ( 'NONE', *, *, #2996, .F. ) ;
#10075 = DIRECTION ( 'NONE',  ( -1.000000000000000000, -0.000000000000000000, -0.000000000000000000 ) ) ;
#10076 = COLOUR_RGB ( '', 0.09019608, 0.27058824, 0.51372549) ;
#10077 = PLANE ( 'NONE',  #7272 ) ;
#10078 = ORIENTED_EDGE ( 'NONE', *, *, #3622, .T. ) ;
#10079 = EDGE_CURVE ( 'NONE', #8384, #8371, #1078, .T. ) ;
#10080 = CYLINDRICAL_SURFACE ( 'NONE', #1010, 3.000000000000000000 ) ;
#10081 = LINE ( 'NONE', #6233, #2620 ) ;
#10082 = CARTESIAN_POINT ( 'NONE',  ( 10.00000000000000000, -8.497168642645966941, 0.2193742428684610779 ) ) ;
#10083 = CARTESIAN_POINT ( 'NONE',  ( 4.023224611898322145, -4.155232146225737111, -0.2960517167220233503 ) ) ;
#10084 = ORIENTED_EDGE ( 'NONE', *, *, #1069, .T. ) ;
#10085 = AXIS2_PLACEMENT_3D ( 'NONE', #157, #3441, #9921 ) ;
#10086 = CARTESIAN_POINT ( 'NONE',  ( 7.054542135639013677E-15, -28.99999999999999289, 0.000000000000000000 ) ) ;
#10087 = CARTESIAN_POINT ( 'NONE',  ( -5.152728359536494551, -2.625446233515535077, 9.939999999999994174 ) ) ;
#10088 = AXIS2_PLACEMENT_3D ( 'NONE', #202, #8312, #2683 ) ;
#10089 = CARTESIAN_POINT ( 'NONE',  ( -1.499999999999999778, -12.13397459621556784, 0.1458333319677399265 ) ) ;
#10090 = CARTESIAN_POINT ( 'NONE',  ( 1.500000000000000222, -13.00000000000000533, -3.000000000000000000 ) ) ;
#10091 = VECTOR ( 'NONE', #4488, 1000.000000000000000 ) ;
#10092 = LINE ( 'NONE', #7905, #2807 ) ;
#10093 = DIRECTION ( 'NONE',  ( 0.000000000000000000, -1.000000000000000000, 0.000000000000000000 ) ) ;
#10094 = LINE ( 'NONE', #1924, #9481 ) ;
#10095 = CARTESIAN_POINT ( 'NONE',  ( 4.430710083317573655, 0.7916369971161595354, 12.47605171672202218 ) ) ;
#10096 = CARTESIAN_POINT ( 'NONE',  ( 8.692241771943169307E-17, -11.58044919106553294, -2.593750000682796486 ) ) ;
#10097 = AXIS2_PLACEMENT_3D ( 'NONE', #9184, #3558, #6785 ) ;
#10098 = CARTESIAN_POINT ( 'NONE',  ( -2.417848759854264618, 4.940838830814694660, 1.243948283277976463 ) ) ;
#10099 = CARTESIAN_POINT ( 'NONE',  ( -0.6146835312500006365, -14.06466310670085562, -1.885416667349463227 ) ) ;
#10100 = AXIS2_PLACEMENT_3D ( 'NONE', #6796, #7654, #10052 ) ;
#10101 = EDGE_LOOP ( 'NONE', ( #1892, #6272, #3783, #5324 ) ) ;
#10102 = DIRECTION ( 'NONE',  ( -1.000000000000000000, 0.000000000000000000, -0.000000000000000000 ) ) ;
#10103 = DIRECTION ( 'NONE',  ( 0.000000000000000000, 0.000000000000000000, -1.000000000000000000 ) ) ;
#10104 = PLANE ( 'NONE',  #9330 ) ;
#10105 = ORIENTED_EDGE ( 'NONE', *, *, #2457, .F. ) ;
#10106 = CIRCLE ( 'NONE', #5518, 2.000000000000000000 ) ;
#10107 = CARTESIAN_POINT ( 'NONE',  ( -3.181980515339458027, -3.181980515339470905, 12.59999999999999787 ) ) ;
#10108 = EDGE_CURVE ( 'NONE', #6004, #4105, #7847, .T. ) ;
#10109 = CARTESIAN_POINT ( 'NONE',  ( 4.215868657802586128, 2.148092372876346801, 2.939999999999999059 ) ) ;
#10110 =( BOUNDED_SURFACE ( )  B_SPLINE_SURFACE ( 1, 2, ( 
 ( #9132, #5983, #8397, #10096, #6728, #5200, #2619, #10047, #5257, #6686, #9088, #334, #2770, #3612, #1076, #9241, #1229, #1822, #4298, #2030, #3665, #1874, #5882, #7649, #4249, #439, #2823, #7543, #8294, #1020, #289, #3512, #7494, #9992, #2667, #5149, #5936, #4351, #1128, #6036, #7591, #1980, #3562, #9889, #1176, #9289, #8498, #4454, #6095, #1438, #10248, #2183, #3819, #2081, #3083, #4508, #6893, #2928, #6996, #5307, #9454, #5460, #8597, #2239, #8699, #1282, #639, #9509, #1328, #2981, #700, #4558, #7048 ),
 ( #6200, #4662, #7806, #9397, #5407, #7854, #10202, #3870, #8548, #588, #10146, #7102, #8650, #7753, #6147, #4610, #9347, #7908, #3029, #2870, #10359, #487, #1386, #6303, #3714, #540, #3767, #10300, #9562, #6945, #6250, #2134, #5356, #2289, #5515, #4714, #8753, #1492, #7963, #2399, #8124, #910, #8864, #3134, #9722, #860, #9669, #3189, #6410, #66, #2453, #4136, #806, #9775, #7156, #4089, #9823, #8020, #10413, #4879, #7323, #4937, #5619, #3292, #5771, #6362, #1605, #6571, #8232, #4828, #10470, #8964, #8809 ) ),
 .UNSPECIFIED., .F., .F., .T. ) 
 B_SPLINE_SURFACE_WITH_KNOTS ( ( 2, 2 ),
 ( 3, 2, 2, 2, 2, 2, 2, 2, 2, 2, 2, 2, 2, 2, 2, 2, 2, 2, 2, 2, 2, 2, 2, 2, 2, 2, 2, 2, 2, 2, 2, 2, 2, 2, 2, 2, 3 ),
 ( 0.000000000000000000, 1.000000000000000000 ),
 ( 0.000000000000000000, 0.02777777777777777624, 0.05555555555555555247, 0.08333333333333332871, 0.1111111111111111049, 0.1388888888888888951, 0.1666666666666666574, 0.1944444444444444475, 0.2222222222222222099, 0.2500000000000000000, 0.2777777777777777901, 0.3055555555555555802, 0.3333333333333333148, 0.3611111111111111049, 0.3888888888888888951, 0.4166666666666666852, 0.4444444444444444198, 0.4722222222222222099, 0.5000000000000000000, 0.5277777777777777901, 0.5555555555555555802, 0.5833333333333333703, 0.6111111111111111605, 0.6388888888888888395, 0.6666666666666666297, 0.6944444444444444198, 0.7222222222222222099, 0.7500000000000000000, 0.7777777777777777901, 0.8055555555555555802, 0.8333333333333333703, 0.8611111111111111605, 0.8888888888888888395, 0.9166666666666666297, 0.9444444444444444198, 0.9722222222222222099, 1.000000000000000000 ),
 .UNSPECIFIED. ) 
 GEOMETRIC_REPRESENTATION_ITEM ( )  RATIONAL_B_SPLINE_SURFACE ( (
 ( 1.000000000000000000, 0.8660254037844387076, 1.000000000000000000, 0.8660254037844387076, 1.000000000000000000, 0.8660254037844387076, 1.000000000000000000, 0.8660254037844387076, 1.000000000000000000, 0.8660254037844387076, 1.000000000000000000, 0.8660254037844387076, 1.000000000000000000, 0.8660254037844387076, 1.000000000000000000, 0.8660254037844387076, 1.000000000000000000, 0.8660254037844387076, 1.000000000000000000, 0.8660254037844387076, 1.000000000000000000, 0.8660254037844387076, 1.000000000000000000, 0.8660254037844387076, 1.000000000000000000, 0.8660254037844387076, 1.000000000000000000, 0.8660254037844387076, 1.000000000000000000, 0.8660254037844387076, 1.000000000000000000, 0.8660254037844387076, 1.000000000000000000, 0.8660254037844387076, 1.000000000000000000, 0.8660254037844387076, 1.000000000000000000, 0.8660254037844387076, 1.000000000000000000, 0.8660254037844387076, 1.000000000000000000, 0.8660254037844387076, 1.000000000000000000, 0.8660254037844387076, 1.000000000000000000, 0.8660254037844387076, 1.000000000000000000, 0.8660254037844387076, 1.000000000000000000, 0.8660254037844387076, 1.000000000000000000, 0.8660254037844387076, 1.000000000000000000, 0.8660254037844387076, 1.000000000000000000, 0.8660254037844387076, 1.000000000000000000, 0.8660254037844387076, 1.000000000000000000, 0.8660254037844387076, 1.000000000000000000, 0.8660254037844387076, 1.000000000000000000, 0.8660254037844387076, 1.000000000000000000, 0.8660254037844387076, 1.000000000000000000, 0.8660254037844387076, 1.000000000000000000, 0.8660254037844387076, 1.000000000000000000, 0.8660254037844387076, 1.000000000000000000),
 ( 1.000000000000000000, 0.8660254037844387076, 1.000000000000000000, 0.8660254037844387076, 1.000000000000000000, 0.8660254037844387076, 1.000000000000000000, 0.8660254037844387076, 1.000000000000000000, 0.8660254037844387076, 1.000000000000000000, 0.8660254037844387076, 1.000000000000000000, 0.8660254037844387076, 1.000000000000000000, 0.8660254037844387076, 1.000000000000000000, 0.8660254037844387076, 1.000000000000000000, 0.8660254037844387076, 1.000000000000000000, 0.8660254037844387076, 1.000000000000000000, 0.8660254037844387076, 1.000000000000000000, 0.8660254037844387076, 1.000000000000000000, 0.8660254037844387076, 1.000000000000000000, 0.8660254037844387076, 1.000000000000000000, 0.8660254037844387076, 1.000000000000000000, 0.8660254037844387076, 1.000000000000000000, 0.8660254037844387076, 1.000000000000000000, 0.8660254037844387076, 1.000000000000000000, 0.8660254037844387076, 1.000000000000000000, 0.8660254037844387076, 1.000000000000000000, 0.8660254037844387076, 1.000000000000000000, 0.8660254037844387076, 1.000000000000000000, 0.8660254037844387076, 1.000000000000000000, 0.8660254037844387076, 1.000000000000000000, 0.8660254037844387076, 1.000000000000000000, 0.8660254037844387076, 1.000000000000000000, 0.8660254037844387076, 1.000000000000000000, 0.8660254037844387076, 1.000000000000000000, 0.8660254037844387076, 1.000000000000000000, 0.8660254037844387076, 1.000000000000000000, 0.8660254037844387076, 1.000000000000000000, 0.8660254037844387076, 1.000000000000000000, 0.8660254037844387076, 1.000000000000000000, 0.8660254037844387076, 1.000000000000000000, 0.8660254037844387076, 1.000000000000000000) ) ) 
 REPRESENTATION_ITEM ( '' )  SURFACE ( )  );
#10111 = CARTESIAN_POINT ( 'NONE',  ( 1.229367062499999719, -13.70977540446724063, 0.1145833326505365929 ) ) ;
#10112 = EDGE_LOOP ( 'NONE', ( #8820, #1463, #9015, #6971, #3526, #3680, #8256, #2774, #9305, #1907, #5715, #7087, #2848, #6714, #1353, #6073, #8416, #7458, #739, #2881, #6320, #4865, #9908, #1401, #9410, #4518, #6844, #5748, #4088, #5804, #6542, #1214, #6313, #563, #1457, #9668, #35, #9257, #2201, #7078, #8566, #962, #7865, #10078, #413, #2008 ) ) ;
#10113 = SURFACE_STYLE_FILL_AREA ( #1044 ) ;
#10114 = ADVANCED_FACE ( 'NONE', ( #8341 ), #6520, .F. ) ;
#10115 = EDGE_LOOP ( 'NONE', ( #3832, #10439, #4635, #2429 ) ) ;
#10116 = DIRECTION ( 'NONE',  ( 0.000000000000000000, 0.000000000000000000, -1.000000000000000000 ) ) ;
#10117 = CARTESIAN_POINT ( 'NONE',  ( 10.00000000000000000, 2.871924938129970517, -6.435996203144478400 ) ) ;
#10118 = DIRECTION ( 'NONE',  ( -0.000000000000000000, 1.000000000000000000, 1.224646799147353207E-16 ) ) ;
#10119 = EDGE_LOOP ( 'NONE', ( #6561, #1653, #7741, #6188 ) ) ;
#10120 = CARTESIAN_POINT ( 'NONE',  ( 0.8603895577212593571, 5.432285873273261068, 10.91999999999999993 ) ) ;
#10121 = CARTESIAN_POINT ( 'NONE',  ( -3.889087296526005044, -3.889087296526019255, 12.59999999999999787 ) ) ;
#10122 = CARTESIAN_POINT ( 'NONE',  ( -0.8603895577212598011, -5.432285873273260179, 9.519999999999999574 ) ) ;
#10123 = ORIENTED_EDGE ( 'NONE', *, *, #8044, .F. ) ;
#10124 = CARTESIAN_POINT ( 'NONE',  ( 19.29399126966725575, 3.750000000000000000, 0.000000000000000000 ) ) ;
#10125 = UNCERTAINTY_MEASURE_WITH_UNIT (LENGTH_MEASURE( 1.000000000000000082E-05 ), #6125, 'distance_accuracy_value', 'NONE');
#10126 = EDGE_CURVE ( 'NONE', #3277, #4919, #1656, .T. ) ;
#10127 = EDGE_CURVE ( 'NONE', #8717, #4944, #70, .T. ) ;
#10128 = VERTEX_POINT ( 'NONE', #8128 ) ;
#10129 = DIRECTION ( 'NONE',  ( 0.000000000000000000, 0.000000000000000000, 1.000000000000000000 ) ) ;
#10130 = LINE ( 'NONE', #9326, #8623 ) ;
#10131 = ORIENTED_EDGE ( 'NONE', *, *, #10200, .F. ) ;
#10132 = DIRECTION ( 'NONE',  ( -1.000000000000000000, 0.000000000000000000, 0.000000000000000000 ) ) ;
#10133 = FACE_OUTER_BOUND ( 'NONE', #3958, .T. ) ;
#10134 = FACE_OUTER_BOUND ( 'NONE', #10178, .T. ) ;
#10135 = CARTESIAN_POINT ( 'NONE',  ( 0.6479879772514793856, -4.687928535947285091, 8.383948283277975477 ) ) ;
#10136 = ORIENTED_EDGE ( 'NONE', *, *, #2803, .F. ) ;
#10137 = CARTESIAN_POINT ( 'NONE',  ( 1.500000000000000444, -12.13397459621556607, -2.520833334698926897 ) ) ;
#10138 = CARTESIAN_POINT ( 'NONE',  ( -2.496947748567517333, 4.900535883036019058, 10.63999999999999879 ) ) ;
#10139 = EDGE_CURVE ( 'NONE', #8579, #5860, #1711, .T. ) ;
#10140 = CARTESIAN_POINT ( 'NONE',  ( -2.000000000000000000, 0.000000000000000000, 0.000000000000000000 ) ) ;
#10141 = CARTESIAN_POINT ( 'NONE',  ( 9.869213319667256457, 3.750000000000000000, -12.00000000000000000 ) ) ;
#10142 = DIRECTION ( 'NONE',  ( 0.000000000000000000, 0.000000000000000000, 1.000000000000000000 ) ) ;
#10143 = DIRECTION ( 'NONE',  ( 1.000000000000000000, 0.000000000000000000, 0.000000000000000000 ) ) ;
#10144 = CARTESIAN_POINT ( 'NONE',  ( -29.99999999999998934, -13.00000000000000533, 0.000000000000000000 ) ) ;
#10145 = CARTESIAN_POINT ( 'NONE',  ( 4.173491630687861331, 2.231261971483781359, 12.33605171672202339 ) ) ;
#10146 = CARTESIAN_POINT ( 'NONE',  ( 0.6146835312499993043, -14.06466310670085562, -2.427083334016129967 ) ) ;
#10147 = CARTESIAN_POINT ( 'NONE',  ( -4.860232935257354114, 2.576046737280751842, 3.763948283277976703 ) ) ;
#10148 = EDGE_CURVE ( 'NONE', #7882, #8371, #7377, .T. ) ;
#10149 = LINE ( 'NONE', #4831, #7337 ) ;
#10150 = ORIENTED_EDGE ( 'NONE', *, *, #5357, .T. ) ;
#10151 = DIRECTION ( 'NONE',  ( 0.000000000000000000, 0.4999999999999991673, -0.8660254037844391517 ) ) ;
#10152 = TOROIDAL_SURFACE ( 'NONE', #5563, 1.600000000000000311, 0.1000000000000000056 ) ;
#10153 = LINE ( 'NONE', #4564, #6270 ) ;
#10154 = DIRECTION ( 'NONE',  ( 0.000000000000000000, 0.000000000000000000, 1.000000000000000000 ) ) ;
#10155 = LINE ( 'NONE', #5157, #7470 ) ;
#10156 = ORIENTED_EDGE ( 'NONE', *, *, #3828, .F. ) ;
#10157 = CARTESIAN_POINT ( 'NONE',  ( -2.042957248827969252, 4.009529358847651714, 13.43999999999999950 ) ) ;
#10158 =( NAMED_UNIT ( * ) SI_UNIT ( $, .STERADIAN. ) SOLID_ANGLE_UNIT ( ) );
#10159 = CARTESIAN_POINT ( 'NONE',  ( -4.430710083317573655, -0.7916369971161599794, 13.87605171672202253 ) ) ;
#10160 = VECTOR ( 'NONE', #3650, 1000.000000000000000 ) ;
#10161 = CARTESIAN_POINT ( 'NONE',  ( -0.6146835312499998594, -11.93533689329915326, -1.177083334016129967 ) ) ;
#10162 = ORIENTED_EDGE ( 'NONE', *, *, #3649, .F. ) ;
#10163 = VERTEX_POINT ( 'NONE', #5670 ) ;
#10164 = CARTESIAN_POINT ( 'NONE',  ( 8.000000000000001776, 5.793104693147763662, 2.343061888689530026 ) ) ;
#10165 = DIRECTION ( 'NONE',  ( -1.000000000000000000, 0.000000000000000000, 0.000000000000000000 ) ) ;
#10166 = FACE_OUTER_BOUND ( 'NONE', #7706, .T. ) ;
#10167 = ORIENTED_EDGE ( 'NONE', *, *, #6493, .F. ) ;
#10168 = AXIS2_PLACEMENT_3D ( 'NONE', #2106, #5331, #7830 ) ;
#10169 = CARTESIAN_POINT ( 'NONE',  ( 0.9968613283357860011, -5.697241258616382531, 10.37605171672202253 ) ) ;
#10170 = CARTESIAN_POINT ( 'NONE',  ( 4.900535883036028828, -2.496947748567499126, 11.75999999999999979 ) ) ;
#10171 = DIRECTION ( 'NONE',  ( 0.000000000000000000, 1.000000000000000000, -7.228014483236699822E-18 ) ) ;
#10172 = EDGE_LOOP ( 'NONE', ( #8656, #9898, #7346, #3018 ) ) ;
#10173 = DIRECTION ( 'NONE',  ( -0.3420201433256627732, 0.9396926207859105373, 0.000000000000000000 ) ) ;
#10174 = EDGE_CURVE ( 'NONE', #10267, #2046, #1414, .T. ) ;
#10175 = AXIS2_PLACEMENT_3D ( 'NONE', #6007, #10118, #6864 ) ;
#10176 = ORIENTED_EDGE ( 'NONE', *, *, #7995, .F. ) ;
#10177 = AXIS2_PLACEMENT_3D ( 'NONE', #3617, #7707, #6845 ) ;
#10178 = EDGE_LOOP ( 'NONE', ( #8933, #1575, #6052, #4870 ) ) ;
#10179 = VECTOR ( 'NONE', #1066, 1000.000000000000000 ) ;
#10180 = CARTESIAN_POINT ( 'NONE',  ( 0.000000000000000000, -10.00000000000000000, -12.00000000000000000 ) ) ;
#10181 = DIRECTION ( 'NONE',  ( 0.3420201433256627732, -0.9396926207859105373, 0.000000000000000000 ) ) ;
#10182 = VECTOR ( 'NONE', #9662, 1000.000000000000000 ) ;
#10183 = ORIENTED_EDGE ( 'NONE', *, *, #6350, .T. ) ;
#10184 = DIRECTION ( 'NONE',  ( 0.000000000000000000, 0.000000000000000000, 1.000000000000000000 ) ) ;
#10185 = VECTOR ( 'NONE', #6528, 1000.000000000000000 ) ;
#10186 = PLANE ( 'NONE',  #4815 ) ;
#10187 = CARTESIAN_POINT ( 'NONE',  ( -4.458484982038663169, -0.6162731882459353550, 6.283948283277974944 ) ) ;
#10188 = VERTEX_POINT ( 'NONE', #9079 ) ;
#10189 = FACE_OUTER_BOUND ( 'NONE', #8428, .T. ) ;
#10190 = EDGE_CURVE ( 'NONE', #2911, #5053, #6467, .T. ) ;
#10191 = VECTOR ( 'NONE', #3754, 1000.000000000000000 ) ;
#10192 = VECTOR ( 'NONE', #5268, 1000.000000000000000 ) ;
#10193 = CARTESIAN_POINT ( 'NONE',  ( -1.500000000000000222, -13.00000000000000533, 0.1874999986344063341 ) ) ;
#10194 = CARTESIAN_POINT ( 'NONE',  ( -0.8603895577212598011, -5.432285873273260179, 12.31999999999999851 ) ) ;
#10195 = CARTESIAN_POINT ( 'NONE',  ( 3.181980515339458471, 3.181980515339470461, 13.99999999999999822 ) ) ;
#10196 = DIRECTION ( 'NONE',  ( -0.000000000000000000, -0.000000000000000000, 1.000000000000000000 ) ) ;
#10197 = PLANE ( 'NONE',  #6697 ) ;
#10198 = CARTESIAN_POINT ( 'NONE',  ( 10.00000000000000000, 1.418488851014483076, -6.085876303339363247 ) ) ;
#10199 = CARTESIAN_POINT ( 'NONE',  ( -4.687928535947287756, 0.6479879772514611780, 11.21605171672202417 ) ) ;
#10200 = EDGE_CURVE ( 'NONE', #7188, #8379, #6998, .T. ) ;
#10201 = EDGE_CURVE ( 'NONE', #6622, #6819, #576, .T. ) ;
#10202 = CARTESIAN_POINT ( 'NONE',  ( -1.229367062500000163, -13.00000000000000533, -2.593750000682796486 ) ) ;
#10203 = CARTESIAN_POINT ( 'NONE',  ( 0.9480714621563713917, 5.418398423912717199, 4.323948283277975868 ) ) ;
#10204 = CARTESIAN_POINT ( 'NONE',  ( 8.692241771943170539E-17, -11.58044919106553650, -0.5937500006827968191 ) ) ;
#10205 = VERTEX_POINT ( 'NONE', #6573 ) ;
#10206 = LINE ( 'NONE', #8601, #2884 ) ;
#10207 = DIRECTION ( 'NONE',  ( 0.3420201433256627732, 0.9396926207859105373, 0.000000000000000000 ) ) ;
#10208 = DIRECTION ( 'NONE',  ( -1.000000000000000000, -0.000000000000000000, -0.000000000000000000 ) ) ;
#10209 = CARTESIAN_POINT ( 'NONE',  ( 8.161409553233806236, -10.00000000000000000, 0.000000000000000000 ) ) ;
#10210 = ORIENTED_EDGE ( 'NONE', *, *, #6737, .F. ) ;
#10211 = EDGE_CURVE ( 'NONE', #4442, #2276, #9826, .T. ) ;
#10212 = DIRECTION ( 'NONE',  ( 1.000000000000000000, 0.000000000000000000, 0.000000000000000000 ) ) ;
#10213 = LINE ( 'NONE', #7821, #3228 ) ;
#10214 = CARTESIAN_POINT ( 'NONE',  ( 0.8323763977770604061, -4.658724279160015413, 13.17605171672201969 ) ) ;
#10215 = CARTESIAN_POINT ( 'NONE',  ( -1.229367062500000163, -13.00000000000000533, -0.5937500006827968191 ) ) ;
#10216 = ORIENTED_EDGE ( 'NONE', *, *, #2362, .T. ) ;
#10217 = ORIENTED_EDGE ( 'NONE', *, *, #7626, .T. ) ;
#10218 = CARTESIAN_POINT ( 'NONE',  ( 8.000000000000001776, 0.000000000000000000, 0.000000000000000000 ) ) ;
#10219 = AXIS2_PLACEMENT_3D ( 'NONE', #3351, #813, #6578 ) ;
#10220 = CARTESIAN_POINT ( 'NONE',  ( 15.00000000000000000, 19.99999999999999645, 6.000000000000000000 ) ) ;
#10221 = ORIENTED_EDGE ( 'NONE', *, *, #5695, .F. ) ;
#10222 = CARTESIAN_POINT ( 'NONE',  ( -4.940838830814703542, 2.417848759854245078, 8.556051716722022249 ) ) ;
#10223 = DIRECTION ( 'NONE',  ( 0.000000000000000000, 0.000000000000000000, 1.000000000000000000 ) ) ;
#10224 = VERTEX_POINT ( 'NONE', #1760 ) ;
#10225 = CARTESIAN_POINT ( 'NONE',  ( 20.72778015323380529, -10.00000000000000000, -12.00000000000000000 ) ) ;
#10226 = PRODUCT_RELATED_PRODUCT_CATEGORY ( 'part', '', ( #7746 ) ) ;
#10227 = ORIENTED_EDGE ( 'NONE', *, *, #4084, .T. ) ;
#10228 = AXIS2_PLACEMENT_3D ( 'NONE', #9799, #8260, #1788 ) ;
#10229 = ORIENTED_EDGE ( 'NONE', *, *, #1247, .T. ) ;
#10230 = CARTESIAN_POINT ( 'NONE',  ( 3.099999999999998757, 0.000000000000000000, 0.000000000000000000 ) ) ;
#10231 = CARTESIAN_POINT ( 'NONE',  ( -2.000000000000012879, 15.00000000000000355, 3.999999999999986233 ) ) ;
#10232 = EDGE_CURVE ( 'NONE', #3542, #8622, #4989, .T. ) ;
#10233 = VERTEX_POINT ( 'NONE', #7425 ) ;
#10234 = CARTESIAN_POINT ( 'NONE',  ( 10.00000000000000000, -7.063614741696270016, 8.843061888689529582 ) ) ;
#10235 = FACE_OUTER_BOUND ( 'NONE', #1678, .T. ) ;
#10236 = CARTESIAN_POINT ( 'NONE',  ( 5.697241258616385196, -0.9968613283357656840, 2.223948283277975779 ) ) ;
#10237 = ORIENTED_EDGE ( 'NONE', *, *, #985, .T. ) ;
#10238 = CARTESIAN_POINT ( 'NONE',  ( 0.7500000000000003331, -11.70096189432334732, -2.479166668032260379 ) ) ;
#10239 = FACE_OUTER_BOUND ( 'NONE', #7671, .T. ) ;
#10240 = CARTESIAN_POINT ( 'NONE',  ( 25.00000000000000000, 3.750000000000000000, 0.000000000000000000 ) ) ;
#10241 = CARTESIAN_POINT ( 'NONE',  ( 1.500000000000000222, -12.13397459621556784, -2.958333333333333037 ) ) ;
#10242 = EDGE_CURVE ( 'NONE', #2444, #7878, #9735, .T. ) ;
#10243 = DIRECTION ( 'NONE',  ( -0.000000000000000000, 1.000000000000000000, -0.000000000000000000 ) ) ;
#10244 = FACE_BOUND ( 'NONE', #2404, .T. ) ;
#10245 = DIRECTION ( 'NONE',  ( -1.000000000000000000, -1.156482317317871478E-16, 5.204170427930421283E-15 ) ) ;
#10246 = CARTESIAN_POINT ( 'NONE',  ( 17.00000000000000000, 19.99999999999999645, -9.000000000000000000 ) ) ;
#10247 = CARTESIAN_POINT ( 'NONE',  ( -3.345732310141667831, 3.345732310141653620, 10.50000000000000000 ) ) ;
#10248 = CARTESIAN_POINT ( 'NONE',  ( 0.6146835312500001924, -11.93533689329915326, -0.6354166673494632267 ) ) ;
#10249 = COLOUR_RGB ( '', 0.31764706, 0.68627451, 0.89019608) ;
#10250 = CARTESIAN_POINT ( 'NONE',  ( -0.9480714621563718358, -5.418398423912716311, 5.723948283277976223 ) ) ;
#10251 = CARTESIAN_POINT ( 'NONE',  ( -0.6146835312499998594, -11.93533689329915326, -1.552083334016129967 ) ) ;
#10252 = VECTOR ( 'NONE', #8026, 1000.000000000000000 ) ;
#10253 = VERTEX_POINT ( 'NONE', #4343 ) ;
#10254 = EDGE_CURVE ( 'NONE', #7411, #2729, #7582, .T. ) ;
#10255 = DIRECTION ( 'NONE',  ( -1.000000000000000000, -0.000000000000000000, -0.000000000000000000 ) ) ;
#10256 = EDGE_CURVE ( 'NONE', #7878, #2444, #5309, .T. ) ;
#10257 = EDGE_LOOP ( 'NONE', ( #1727, #6654, #3645, #2084 ) ) ;
#10258 = CARTESIAN_POINT ( 'NONE',  ( 5.999999999999999112, 26.99999999999999289, -4.000000000000000000 ) ) ;
#10259 = CARTESIAN_POINT ( 'NONE',  ( 10.71950000000001424, 1.836970198721030181E-16, -1.500000000000000222 ) ) ;
#10260 = DIRECTION ( 'NONE',  ( 0.000000000000000000, 0.000000000000000000, 1.000000000000000000 ) ) ;
#10261 = ORIENTED_EDGE ( 'NONE', *, *, #8272, .T. ) ;
#10262 = AXIS2_PLACEMENT_3D ( 'NONE', #8104, #3429, #944 ) ;
#10263 = CARTESIAN_POINT ( 'NONE',  ( -2.000000000000000000, 4.561279057474473930, -4.271385531633122845 ) ) ;
#10264 = AXIS2_PLACEMENT_3D ( 'NONE', #2766, #6787, #5980 ) ;
#10265 = CARTESIAN_POINT ( 'NONE',  ( -4.673326407553653361, 0.7401821875142517992, 13.01999999999999424 ) ) ;
#10266 = CARTESIAN_POINT ( 'NONE',  ( -1.229367062500000163, -12.29022459553277002, -0.1354166673494631989 ) ) ;
#10267 = VERTEX_POINT ( 'NONE', #5141 ) ;
#10268 = ADVANCED_FACE ( 'NONE', ( #432 ), #1120, .F. ) ;
#10269 = VECTOR ( 'NONE', #10142, 1000.000000000000000 ) ;
#10270 = VERTEX_POINT ( 'NONE', #5348 ) ;
#10271 = AXIS2_PLACEMENT_3D ( 'NONE', #10297, #2285, #5509 ) ;
#10272 = CARTESIAN_POINT ( 'NONE',  ( -0.000000000000000000, -4.000000000000000000, -2.000000000000000000 ) ) ;
#10273 =( LENGTH_UNIT ( ) NAMED_UNIT ( * ) SI_UNIT ( .MILLI., .METRE. ) );
#10274 = ORIENTED_EDGE ( 'NONE', *, *, #2792, .F. ) ;
#10275 = CARTESIAN_POINT ( 'NONE',  ( -2.542276634908081423, -5.195105386651227342, 10.65605171672202012 ) ) ;
#10276 = CARTESIAN_POINT ( 'NONE',  ( 12.12193523033274545, -7.750000000000000000, -12.00000000000000000 ) ) ;
#10277 = EDGE_LOOP ( 'NONE', ( #10054, #296, #683, #4354 ) ) ;
#10278 = CARTESIAN_POINT ( 'NONE',  ( 1.500000000000000222, -13.00000000000000533, -1.562500001365593416 ) ) ;
#10279 = EDGE_LOOP ( 'NONE', ( #4119, #10390, #1080, #4062 ) ) ;
#10280 = EDGE_CURVE ( 'NONE', #7779, #1248, #479, .T. ) ;
#10281 = VERTEX_POINT ( 'NONE', #1321 ) ;
#10282 = FACE_OUTER_BOUND ( 'NONE', #7255, .T. ) ;
#10283 = CYLINDRICAL_SURFACE ( 'NONE', #6425, 2.750000000000000000 ) ;
#10284 = ORIENTED_EDGE ( 'NONE', *, *, #1304, .F. ) ;
#10285 = CARTESIAN_POINT ( 'NONE',  ( 4.000000000000000000, -13.00000000000000533, 0.000000000000000000 ) ) ;
#10286 = DIRECTION ( 'NONE',  ( 0.000000000000000000, 0.000000000000000000, -1.000000000000000000 ) ) ;
#10287 = CARTESIAN_POINT ( 'NONE',  ( -5.195105386651219348, -2.542276634908102295, 6.143948283277977040 ) ) ;
#10288 = ORIENTED_EDGE ( 'NONE', *, *, #5583, .T. ) ;
#10289 = CARTESIAN_POINT ( 'NONE',  ( -3.181725716174720498E-16, -14.73205080756888385, -2.187500001365593416 ) ) ;
#10290 = CARTESIAN_POINT ( 'NONE',  ( 4.000000000000000888, -2.417132211460011337, -8.149077976821821778 ) ) ;
#10291 = CARTESIAN_POINT ( 'NONE',  ( 10.68814634676619413, 6.000000000000000000, -12.00000000000000000 ) ) ;
#10292 = PRODUCT ( 'jaw_ISO - Spur gear 1M 15T 20PA 8FW ---S15A75H50L4.0N', 'jaw_ISO - Spur gear 1M 15T 20PA 8FW ---S15A75H50L4.0N', '', ( #2456 ) ) ;
#10293 = CARTESIAN_POINT ( 'NONE',  ( -2.496947748567517333, 4.900535883036019058, 13.43999999999999950 ) ) ;
#10294 = CARTESIAN_POINT ( 'NONE',  ( -31.74999999999995737, 0.000000000000000000, 0.000000000000000000 ) ) ;
#10295 = DIRECTION ( 'NONE',  ( -1.000000000000000000, 0.000000000000000000, 0.000000000000000000 ) ) ;
#10296 = ADVANCED_FACE ( 'NONE', ( #9983, #1166, #1222 ), #8591, .T. ) ;
#10297 = CARTESIAN_POINT ( 'NONE',  ( 9.000000000000000000, 19.99999999999999645, 15.00000000000000000 ) ) ;
#10298 = LINE ( 'NONE', #3711, #3702 ) ;
#10299 = CARTESIAN_POINT ( 'NONE',  ( -2.042957248827969252, 4.009529358847651714, 10.63999999999999879 ) ) ;
#10300 = CARTESIAN_POINT ( 'NONE',  ( 8.692241771943169307E-17, -11.58044919106553294, -1.718750000682796708 ) ) ;
#10301 = EDGE_CURVE ( 'NONE', #5749, #717, #7641, .T. ) ;
#10302 = CARTESIAN_POINT ( 'NONE',  ( 5.195105386651219348, 2.542276634908100075, 4.743948283277974909 ) ) ;
#10303 = CARTESIAN_POINT ( 'NONE',  ( 4.404961046766194599, 6.000000000000000000, -12.00000000000000000 ) ) ;
#10304 = ORIENTED_EDGE ( 'NONE', *, *, #3333, .F. ) ;
#10305 = CARTESIAN_POINT ( 'NONE',  ( 0.000000000000000000, -10.00000000000000000, -12.00000000000000000 ) ) ;
#10306 = LINE ( 'NONE', #9459, #2889 ) ;
#10307 = PLANE ( 'NONE',  #1285 ) ;
#10308 = CARTESIAN_POINT ( 'NONE',  ( 1.500000000000000222, -13.00000000000000533, -1.500000000000000000 ) ) ;
#10309 = ORIENTED_EDGE ( 'NONE', *, *, #9166, .F. ) ;
#10310 = CARTESIAN_POINT ( 'NONE',  ( -2.000000000000024425, 15.00000000000000355, -5.999999999999988454 ) ) ;
#10311 = CARTESIAN_POINT ( 'NONE',  ( -15.00000000000000000, 19.99999999999999645, -9.000000000000000000 ) ) ;
#10312 = CARTESIAN_POINT ( 'NONE',  ( 4.673326407553653361, -0.7401821875142523544, 8.820000000000000284 ) ) ;
#10313 = CARTESIAN_POINT ( 'NONE',  ( -1.500000000000000666, -13.86602540378444459, -2.208333333333333481 ) ) ;
#10314 = VECTOR ( 'NONE', #8017, 999.9999999999998863 ) ;
#10315 = VERTEX_POINT ( 'NONE', #7535 ) ;
#10316 = ORIENTED_EDGE ( 'NONE', *, *, #8493, .F. ) ;
#10317 = DIRECTION ( 'NONE',  ( 0.000000000000000000, 0.000000000000000000, 1.000000000000000000 ) ) ;
#10318 = CARTESIAN_POINT ( 'NONE',  ( -0.7499999999999997780, -11.70096189432334555, -2.395833334698926897 ) ) ;
#10319 = VERTEX_POINT ( 'NONE', #9282 ) ;
#10320 = CARTESIAN_POINT ( 'NONE',  ( -5.110351332421769754, -2.708615832122969191, 13.73605171672202019 ) ) ;
#10321 = VECTOR ( 'NONE', #7387, 1000.000000000000000 ) ;
#10322 = DIRECTION ( 'NONE',  ( -1.000000000000000000, 0.000000000000000000, 0.000000000000000000 ) ) ;
#10323 = FILL_AREA_STYLE ('',( #3845 ) ) ;
#10324 = ORIENTED_EDGE ( 'NONE', *, *, #6732, .F. ) ;
#10325 = EDGE_CURVE ( 'NONE', #8892, #2098, #2581, .T. ) ;
#10326 = AXIS2_PLACEMENT_3D ( 'NONE', #1475, #6344, #2964 ) ;
#10327 = EDGE_CURVE ( 'NONE', #4315, #3824, #6832, .T. ) ;
#10328 = CARTESIAN_POINT ( 'NONE',  ( 23.25451694676619496, -10.00000000000000000, -12.00000000000000000 ) ) ;
#10329 = CARTESIAN_POINT ( 'NONE',  ( 5.726445515403654873, -0.8124729078101852187, 9.816051716722022036 ) ) ;
#10330 = AXIS2_PLACEMENT_3D ( 'NONE', #9782, #9684, #3302 ) ;
#10331 = ORIENTED_EDGE ( 'NONE', *, *, #610, .F. ) ;
#10332 =( NAMED_UNIT ( * ) SI_UNIT ( $, .STERADIAN. ) SOLID_ANGLE_UNIT ( ) );
#10333 = CONICAL_SURFACE ( 'NONE', #3718, 1.249999999999997558, 1.029744258676650981 ) ;
#10334 = ORIENTED_EDGE ( 'NONE', *, *, #1223, .F. ) ;
#10335 = CARTESIAN_POINT ( 'NONE',  ( 5.838749930332745919, 3.750000000000000000, -12.00000000000000000 ) ) ;
#10336 = AXIS2_PLACEMENT_3D ( 'NONE', #5892, #5847, #7602 ) ;
#10337 = CARTESIAN_POINT ( 'NONE',  ( 1.300000000000000044, 1.478016689125442484, -1.626303258728256651E-15 ) ) ;
#10338 = ORIENTED_EDGE ( 'NONE', *, *, #885, .F. ) ;
#10339 = DIRECTION ( 'NONE',  ( -1.000000000000000000, -0.000000000000000000, -0.000000000000000000 ) ) ;
#10340 = LINE ( 'NONE', #1641, #8541 ) ;
#10341 = CARTESIAN_POINT ( 'NONE',  ( 0.8124729078102063129, -5.726445515403652209, 8.383948283277975477 ) ) ;
#10342 = ORIENTED_EDGE ( 'NONE', *, *, #6196, .T. ) ;
#10343 = EDGE_CURVE ( 'NONE', #1958, #4156, #2815, .T. ) ;
#10344 = VECTOR ( 'NONE', #4218, 1000.000000000000000 ) ;
#10345 = CARTESIAN_POINT ( 'NONE',  ( -1.500000000000000222, -13.00000000000000533, -1.812500001365593416 ) ) ;
#10346 = AXIS2_PLACEMENT_3D ( 'NONE', #7230, #3305, #5529 ) ;
#10347 = CARTESIAN_POINT ( 'NONE',  ( 30.00000000000001066, -34.99999999999999289, 9.000000000000000000 ) ) ;
#10348 = DIRECTION ( 'NONE',  ( 0.000000000000000000, 0.5000000000000009992, 0.8660254037844380415 ) ) ;
#10349 = EDGE_LOOP ( 'NONE', ( #1291, #5274, #10, #7561 ) ) ;
#10350 = DIRECTION ( 'NONE',  ( -0.000000000000000000, -0.000000000000000000, -1.000000000000000000 ) ) ;
#10351 = AXIS2_PLACEMENT_3D ( 'NONE', #6957, #9250, #1987 ) ;
#10352 = CARTESIAN_POINT ( 'NONE',  ( 10.00000000000000000, 6.226349476952025341, -0.5315761383463619705 ) ) ;
#10353 = CARTESIAN_POINT ( 'NONE',  ( -1.500000000000003331, -13.86602540378444104, -2.208333333333333481 ) ) ;
#10354 = DIRECTION ( 'NONE',  ( -1.000000000000000000, -0.000000000000000000, -0.000000000000000000 ) ) ;
#10355 = APPLICATION_CONTEXT ( 'automotive_design' ) ;
#10356 = VECTOR ( 'NONE', #2705, 1000.000000000000000 ) ;
#10357 = FACE_OUTER_BOUND ( 'NONE', #141, .T. ) ;
#10358 = CARTESIAN_POINT ( 'NONE',  ( 3.345732310141667387, -3.345732310141653620, 6.299999999999999822 ) ) ;
#10359 = CARTESIAN_POINT ( 'NONE',  ( -0.6146835312500006365, -14.06466310670085562, -2.010416667349463005 ) ) ;
#10360 = AXIS2_PLACEMENT_3D ( 'NONE', #10368, #9296, #4 ) ;
#10361 = CARTESIAN_POINT ( 'NONE',  ( 2.417848759854264618, -4.940838830814695548, 8.243948283277976685 ) ) ;
#10362 = EDGE_CURVE ( 'NONE', #8513, #4283, #6138, .T. ) ;
#10363 = DIRECTION ( 'NONE',  ( 0.000000000000000000, 0.000000000000000000, 1.000000000000000000 ) ) ;
#10364 = ORIENTED_EDGE ( 'NONE', *, *, #3976, .F. ) ;
#10365 = APPLICATION_PROTOCOL_DEFINITION ( 'draft international standard', 'automotive_design', 1998, #9259 ) ;
#10366 = DIRECTION ( 'NONE',  ( -1.000000000000000000, 0.000000000000000000, -0.000000000000000000 ) ) ;
#10367 = DIRECTION ( 'NONE',  ( -1.000000000000000000, -0.000000000000000000, -0.000000000000000000 ) ) ;
#10368 = CARTESIAN_POINT ( 'NONE',  ( 0.000000000000000000, 18.99999999999999289, 0.000000000000000000 ) ) ;
#10369 = DIRECTION ( 'NONE',  ( 0.000000000000000000, 0.000000000000000000, -1.000000000000000000 ) ) ;
#10370 = CARTESIAN_POINT ( 'NONE',  ( 12.99999999999999645, 19.99999999999999645, -9.000000000000000000 ) ) ;
#10371 = ORIENTED_EDGE ( 'NONE', *, *, #7852, .T. ) ;
#10372 = LINE ( 'NONE', #3833, #7948 ) ;
#10373 = DIRECTION ( 'NONE',  ( 0.000000000000000000, 0.000000000000000000, 1.000000000000000000 ) ) ;
#10374 = CARTESIAN_POINT ( 'NONE',  ( -4.215868657802586128, -2.148092372876348133, 9.939999999999994174 ) ) ;
#10375 = UNCERTAINTY_MEASURE_WITH_UNIT (LENGTH_MEASURE( 1.000000000000000082E-05 ), #9434, 'distance_accuracy_value', 'NONE');
#10376 = CARTESIAN_POINT ( 'NONE',  ( -0.7499999999999997780, -11.70096189432334555, -1.833333333333333481 ) ) ;
#10377 = VERTEX_POINT ( 'NONE', #5299 ) ;
#10378 = ORIENTED_EDGE ( 'NONE', *, *, #6981, .F. ) ;
#10379 = CARTESIAN_POINT ( 'NONE',  ( -2.000000000000000000, -6.700937042937071375, 2.183447440113169602 ) ) ;
#10380 = EDGE_CURVE ( 'NONE', #5808, #4718, #1936, .T. ) ;
#10381 = CARTESIAN_POINT ( 'NONE',  ( 20.12216914071655793, -10.02539999999999942, 0.000000000000000000 ) ) ;
#10382 = VERTEX_POINT ( 'NONE', #7694 ) ;
#10383 = CARTESIAN_POINT ( 'NONE',  ( -4.940838830814703542, 2.417848759854245078, 5.756051716722022427 ) ) ;
#10384 = DIRECTION ( 'NONE',  ( 0.3420201433256627732, -0.9396926207859105373, 0.000000000000000000 ) ) ;
#10385 = CYLINDRICAL_SURFACE ( 'NONE', #1855, 1.999999999999997780 ) ;
#10386 = ORIENTED_EDGE ( 'NONE', *, *, #3658, .F. ) ;
#10387 = DIRECTION ( 'NONE',  ( 0.000000000000000000, 0.000000000000000000, 1.000000000000000000 ) ) ;
#10388 = CARTESIAN_POINT ( 'NONE',  ( -3.826313983664925811, -3.951860609387098489, 10.79605171672202246 ) ) ;
#10389 = PRODUCT_DEFINITION_SHAPE ( 'NONE', 'NONE',  #9906 ) ;
#10390 = ORIENTED_EDGE ( 'NONE', *, *, #8236, .F. ) ;
#10391 =( LENGTH_UNIT ( ) NAMED_UNIT ( * ) SI_UNIT ( .MILLI., .METRE. ) );
#10392 = CIRCLE ( 'NONE', #8519, 6.248999999999999666 ) ;
#10393 = EDGE_CURVE ( 'NONE', #5625, #5471, #4130, .T. ) ;
#10394 = PLANE ( 'NONE',  #5836 ) ;
#10395 = EDGE_CURVE ( 'NONE', #3169, #4115, #9499, .T. ) ;
#10396 = DIRECTION ( 'NONE',  ( 0.000000000000000000, 1.000000000000000000, 0.000000000000000000 ) ) ;
#10397 = ORIENTED_EDGE ( 'NONE', *, *, #9829, .F. ) ;
#10398 = LINE ( 'NONE', #3117, #3540 ) ;
#10399 = LINE ( 'NONE', #1951, #4793 ) ;
#10400 = CARTESIAN_POINT ( 'NONE',  ( 0.8124729078102063129, -5.726445515403652209, 5.583948283277975655 ) ) ;
#10401 = EDGE_LOOP ( 'NONE', ( #9470, #4984, #5010, #10324 ) ) ;
#10402 = CARTESIAN_POINT ( 'NONE',  ( 1.060575238724907038E-16, -11.26794919243112680, -0.9375000013655937492 ) ) ;
#10403 = AXIS2_PLACEMENT_3D ( 'NONE', #4560, #3667, #8552 ) ;
#10404 = LINE ( 'NONE', #3756, #7153 ) ;
#10405 = ORIENTED_EDGE ( 'NONE', *, *, #7678, .T. ) ;
#10406 = EDGE_CURVE ( 'NONE', #5555, #1004, #8639, .T. ) ;
#10407 = CARTESIAN_POINT ( 'NONE',  ( 0.000000000000000000, -13.00000000000000533, 2.000000000000000000 ) ) ;
#10408 = CARTESIAN_POINT ( 'NONE',  ( 1.999999999999986233, 15.00000000000000355, -4.000000000000009770 ) ) ;
#10409 = VECTOR ( 'NONE', #8010, 1000.000000000000000 ) ;
#10410 = LINE ( 'NONE', #4658, #115 ) ;
#10411 = CARTESIAN_POINT ( 'NONE',  ( 15.26352788033274699, 3.750000000000000000, 0.000000000000000000 ) ) ;
#10412 = CARTESIAN_POINT ( 'NONE',  ( 4.444597532678119300, 0.7039550926810472786, 8.679999999999997939 ) ) ;
#10413 = CARTESIAN_POINT ( 'NONE',  ( 0.6146835312499993043, -14.06466310670085562, -0.4270833340161298564 ) ) ;
#10414 = CARTESIAN_POINT ( 'NONE',  ( -4.860232935257354114, 2.576046737280751842, 9.363948283277975904 ) ) ;
#10415 = AXIS2_PLACEMENT_3D ( 'NONE', #3751, #3857, #10286 ) ;
#10416 = FACE_OUTER_BOUND ( 'NONE', #3912, .T. ) ;
#10417 = EDGE_LOOP ( 'NONE', ( #1306, #8023 ) ) ;
#10418 =( NAMED_UNIT ( * ) PLANE_ANGLE_UNIT ( ) SI_UNIT ( $, .RADIAN. ) );
#10419 = CARTESIAN_POINT ( 'NONE',  ( -5.432285873273256627, -0.8603895577212797852, 1.679999999999999938 ) ) ;
#10420 = PLANE ( 'NONE',  #7033 ) ;
#10421 = VERTEX_POINT ( 'NONE', #9445 ) ;
#10422 = LINE ( 'NONE', #2192, #604 ) ;
#10423 = CARTESIAN_POINT ( 'NONE',  ( -2.000000000000000000, 5.471841788314748989, -3.018103451449677621 ) ) ;
#10424 = DIRECTION ( 'NONE',  ( 0.3420201433256627732, 0.9396926207859105373, -0.000000000000000000 ) ) ;
#10425 = VECTOR ( 'NONE', #3610, 1000.000000000000000 ) ;
#10426 = CARTESIAN_POINT ( 'NONE',  ( 1.500000000000000222, -13.00000000000000533, -0.06250000136559345776 ) ) ;
#10427 = CARTESIAN_POINT ( 'NONE',  ( 20.72778015323380885, 6.000000000000000000, -12.00000000000000000 ) ) ;
#10428 = CIRCLE ( 'NONE', #7016, 2.000000000000000000 ) ;
#10429 = CARTESIAN_POINT ( 'NONE',  ( 2.148092372876330369, 4.215868657802593233, 13.85999999999999766 ) ) ;
#10430 = CARTESIAN_POINT ( 'NONE',  ( 0.7500000000000003331, -11.70096189432334732, -2.416666666666666963 ) ) ;
#10431 = PRODUCT_DEFINITION_FORMATION_WITH_SPECIFIED_SOURCE ( 'ANY', '', #8938, .NOT_KNOWN. ) ;
#10432 = ORIENTED_EDGE ( 'NONE', *, *, #4198, .T. ) ;
#10433 = EDGE_CURVE ( 'NONE', #5848, #6919, #7145, .T. ) ;
#10434 = ORIENTED_EDGE ( 'NONE', *, *, #5006, .T. ) ;
#10435 = CARTESIAN_POINT ( 'NONE',  ( 17.58618750323380553, 6.000000000000000000, -12.00000000000000000 ) ) ;
#10436 = VECTOR ( 'NONE', #2892, 1000.000000000000000 ) ;
#10437 = LINE ( 'NONE', #2206, #1537 ) ;
#10438 = EDGE_CURVE ( 'NONE', #9594, #10270, #2175, .T. ) ;
#10439 = ORIENTED_EDGE ( 'NONE', *, *, #784, .F. ) ;
#10440 = FACE_OUTER_BOUND ( 'NONE', #3273, .T. ) ;
#10441 = CARTESIAN_POINT ( 'NONE',  ( 8.000000000000001776, -2.652816298622379776, -5.657964889053610946 ) ) ;
#10442 = ORIENTED_EDGE ( 'NONE', *, *, #8813, .T. ) ;
#10443 = DIRECTION ( 'NONE',  ( 0.000000000000000000, 0.000000000000000000, 1.000000000000000000 ) ) ;
#10444 = CARTESIAN_POINT ( 'NONE',  ( -2.122056237541221968, 3.969226411068977889, 3.236051716722023297 ) ) ;
#10445 = VECTOR ( 'NONE', #707, 1000.000000000000000 ) ;
#10446 = EDGE_CURVE ( 'NONE', #9404, #4215, #2972, .T. ) ;
#10447 = ORIENTED_EDGE ( 'NONE', *, *, #8134, .T. ) ;
#10448 = CIRCLE ( 'NONE', #7722, 2.500000000000000000 ) ;
#10449 = ORIENTED_EDGE ( 'NONE', *, *, #9234, .F. ) ;
#10450 = DIRECTION ( 'NONE',  ( 0.3420201433256627732, -0.9396926207859105373, 0.000000000000000000 ) ) ;
#10451 = CARTESIAN_POINT ( 'NONE',  ( 0.7500000000000003331, -11.70096189432334732, -1.916666666666666741 ) ) ;
#10452 = ORIENTED_EDGE ( 'NONE', *, *, #4810, .T. ) ;
#10453 = CARTESIAN_POINT ( 'NONE',  ( 2.625446233515515537, 5.152728359536502545, 2.659999999999998366 ) ) ;
#10454 = DIRECTION ( 'NONE',  ( -1.000000000000000000, -0.000000000000000000, -0.000000000000000000 ) ) ;
#10455 = CARTESIAN_POINT ( 'NONE',  ( -5.446173322633801384, -0.7727076532861678615, 3.483948283277976898 ) ) ;
#10456 = ORIENTED_EDGE ( 'NONE', *, *, #6295, .T. ) ;
#10457 = CARTESIAN_POINT ( 'NONE',  ( 1.229367062500000163, -13.00000000000000533, -2.718750000682796486 ) ) ;
#10458 = CARTESIAN_POINT ( 'NONE',  ( 1.229367062500000385, -12.29022459553277002, -2.302083334016129967 ) ) ;
#10459 = EDGE_CURVE ( 'NONE', #4861, #5532, #6827, .T. ) ;
#10460 =( BOUNDED_CURVE ( )  B_SPLINE_CURVE ( 2, ( #3250, #9029, #4836 ),
 .UNSPECIFIED., .F., .T. ) 
 B_SPLINE_CURVE_WITH_KNOTS ( ( 3, 3 ),
 ( 0.8333333333333332593, 0.8538060088535064374 ),
 .UNSPECIFIED. ) 
 CURVE ( )  GEOMETRIC_REPRESENTATION_ITEM ( )  RATIONAL_B_SPLINE_CURVE ( ( 1.000000000000000444, 0.9012585362943735801, 0.9480652127606681301 ) ) 
 REPRESENTATION_ITEM ( '' )  );
#10461 = CARTESIAN_POINT ( 'NONE',  ( 5.999999999999999112, -27.00000000000000711, -17.00000000000000000 ) ) ;
#10462 = VERTEX_POINT ( 'NONE', #2332 ) ;
#10463 = DIRECTION ( 'NONE',  ( 0.9396926207859105373, -0.3420201433256627732, 0.000000000000000000 ) ) ;
#10464 = FACE_OUTER_BOUND ( 'NONE', #7731, .T. ) ;
#10465 = FACE_OUTER_BOUND ( 'NONE', #2295, .T. ) ;
#10466 = CARTESIAN_POINT ( 'NONE',  ( 6.727620669667255804, 3.750000000000000000, -12.00000000000000000 ) ) ;
#10467 = CARTESIAN_POINT ( 'NONE',  ( 2.039008344562727615, -1.214068345727601445E-18, 0.000000000000000000 ) ) ;
#10468 = CARTESIAN_POINT ( 'NONE',  ( -0.7039550926810301812, -4.444597532678121965, 6.719999999999999751 ) ) ;
#10469 = ORIENTED_EDGE ( 'NONE', *, *, #1624, .T. ) ;
#10470 = CARTESIAN_POINT ( 'NONE',  ( 0.6146835312499993043, -14.06466310670085562, 0.07291666598386974119 ) ) ;
#10471 = VECTOR ( 'NONE', #1126, 1000.000000000000000 ) ;
#10472 = EDGE_CURVE ( 'NONE', #3105, #216, #913, .T. ) ;
#10473 = ADVANCED_FACE ( 'NONE', ( #2231, #7950 ), #580, .F. ) ;
#10474 = CARTESIAN_POINT ( 'NONE',  ( -0.9480714621563718358, -5.418398423912716311, 8.523948283277976046 ) ) ;
#10475 = DIRECTION ( 'NONE',  ( -1.000000000000000000, 0.000000000000000000, 0.000000000000000000 ) ) ;
#10476 = VERTEX_POINT ( 'NONE', #10461 ) ;
#10477 = DIRECTION ( 'NONE',  ( 1.000000000000000000, 0.000000000000000000, 0.000000000000000000 ) ) ;
#10478 = CYLINDRICAL_SURFACE ( 'NONE', #5679, 4.000000000000000000 ) ;
#10479 = ORIENTED_EDGE ( 'NONE', *, *, #6734, .T. ) ;
#10480 = PLANE ( 'NONE',  #3316 ) ;
#10481 = CARTESIAN_POINT ( 'NONE',  ( 1.500000000000000222, -13.00000000000000533, -3.000000000000000000 ) ) ;
#10482 = PLANE ( 'NONE',  #1859 ) ;
#10483 = CARTESIAN_POINT ( 'NONE',  ( 0.000000000000000000, 6.000000000000000000, 0.000000000000000000 ) ) ;
#10484 = DIRECTION ( 'NONE',  ( 0.000000000000000000, 0.000000000000000000, -1.000000000000000000 ) ) ;
#10485 = ADVANCED_FACE ( 'NONE', ( #7844 ), #8798, .T. ) ;
#10486 = CARTESIAN_POINT ( 'NONE',  ( -2.231261971483764484, -4.173491630687871101, 0.2639482832779765920 ) ) ;
#10487 = PRODUCT_DEFINITION_CONTEXT ( 'detailed design', #2562, 'design' ) ;
#10488 = CARTESIAN_POINT ( 'NONE',  ( -0.7499999999999997780, -11.70096189432334555, -0.3333333333333334814 ) ) ;
#10489 = ORIENTED_EDGE ( 'NONE', *, *, #1635, .T. ) ;
#10490 = VERTEX_POINT ( 'NONE', #10240 ) ;
#10491 = CARTESIAN_POINT ( 'NONE',  ( 17.57694265928344635, -10.02539999999999942, -12.00000000000000000 ) ) ;
#10492 = DIRECTION ( 'NONE',  ( -0.3420201433256627732, -0.9396926207859105373, 0.000000000000000000 ) ) ;
#10493 = ORIENTED_EDGE ( 'NONE', *, *, #63, .F. ) ;
#10494 = DIRECTION ( 'NONE',  ( 0.000000000000000000, 0.000000000000000000, -1.000000000000000000 ) ) ;
#10495 = CARTESIAN_POINT ( 'NONE',  ( -5.999999999999999112, -27.00000000000000711, -14.00000000000000178 ) ) ;
#10496 = ORIENTED_EDGE ( 'NONE', *, *, #2305, .F. ) ;
#10497 = CARTESIAN_POINT ( 'NONE',  ( -5.726445515403654873, 0.8124729078101847746, 11.21605171672202417 ) ) ;
#10498 = CARTESIAN_POINT ( 'NONE',  ( -1.500000000000000666, -13.86602540378444459, -0.7708333346989267865 ) ) ;
#10499 = NEXT_ASSEMBLY_USAGE_OCCURRENCE ( 'NAUO1', ' ', ' ', #5214, #3345, $ ) ;
#10500 = NEXT_ASSEMBLY_USAGE_OCCURRENCE ( 'NAUO2', ' ', ' ', #5214, #6123, $ ) ;
#10501 = NEXT_ASSEMBLY_USAGE_OCCURRENCE ( 'NAUO3', ' ', ' ', #5214, #8792, $ ) ;
#10502 = NEXT_ASSEMBLY_USAGE_OCCURRENCE ( 'NAUO4', ' ', ' ', #5214, #3931, $ ) ;
#10503 = NEXT_ASSEMBLY_USAGE_OCCURRENCE ( 'NAUO5', ' ', ' ', #5214, #496, $ ) ;
#10504 = NEXT_ASSEMBLY_USAGE_OCCURRENCE ( 'NAUO6', ' ', ' ', #5214, #9906, $ ) ;
#10505 = NEXT_ASSEMBLY_USAGE_OCCURRENCE ( 'NAUO7', ' ', ' ', #5214, #1276, $ ) ;
#10506 = NEXT_ASSEMBLY_USAGE_OCCURRENCE ( 'NAUO8', ' ', ' ', #5214, #7235, $ ) ;
#10507 = NEXT_ASSEMBLY_USAGE_OCCURRENCE ( 'NAUO9', ' ', ' ', #5214, #4567, $ ) ;
#10508 = NEXT_ASSEMBLY_USAGE_OCCURRENCE ( 'NAUO10', ' ', ' ', #5214, #4567, $ ) ;
#10509 = NEXT_ASSEMBLY_USAGE_OCCURRENCE ( 'NAUO11', ' ', ' ', #5214, #8792, $ ) ;
#10510 = NEXT_ASSEMBLY_USAGE_OCCURRENCE ( 'NAUO12', ' ', ' ', #5214, #6123, $ ) ;
ENDSEC;
END-ISO-10303-21;
